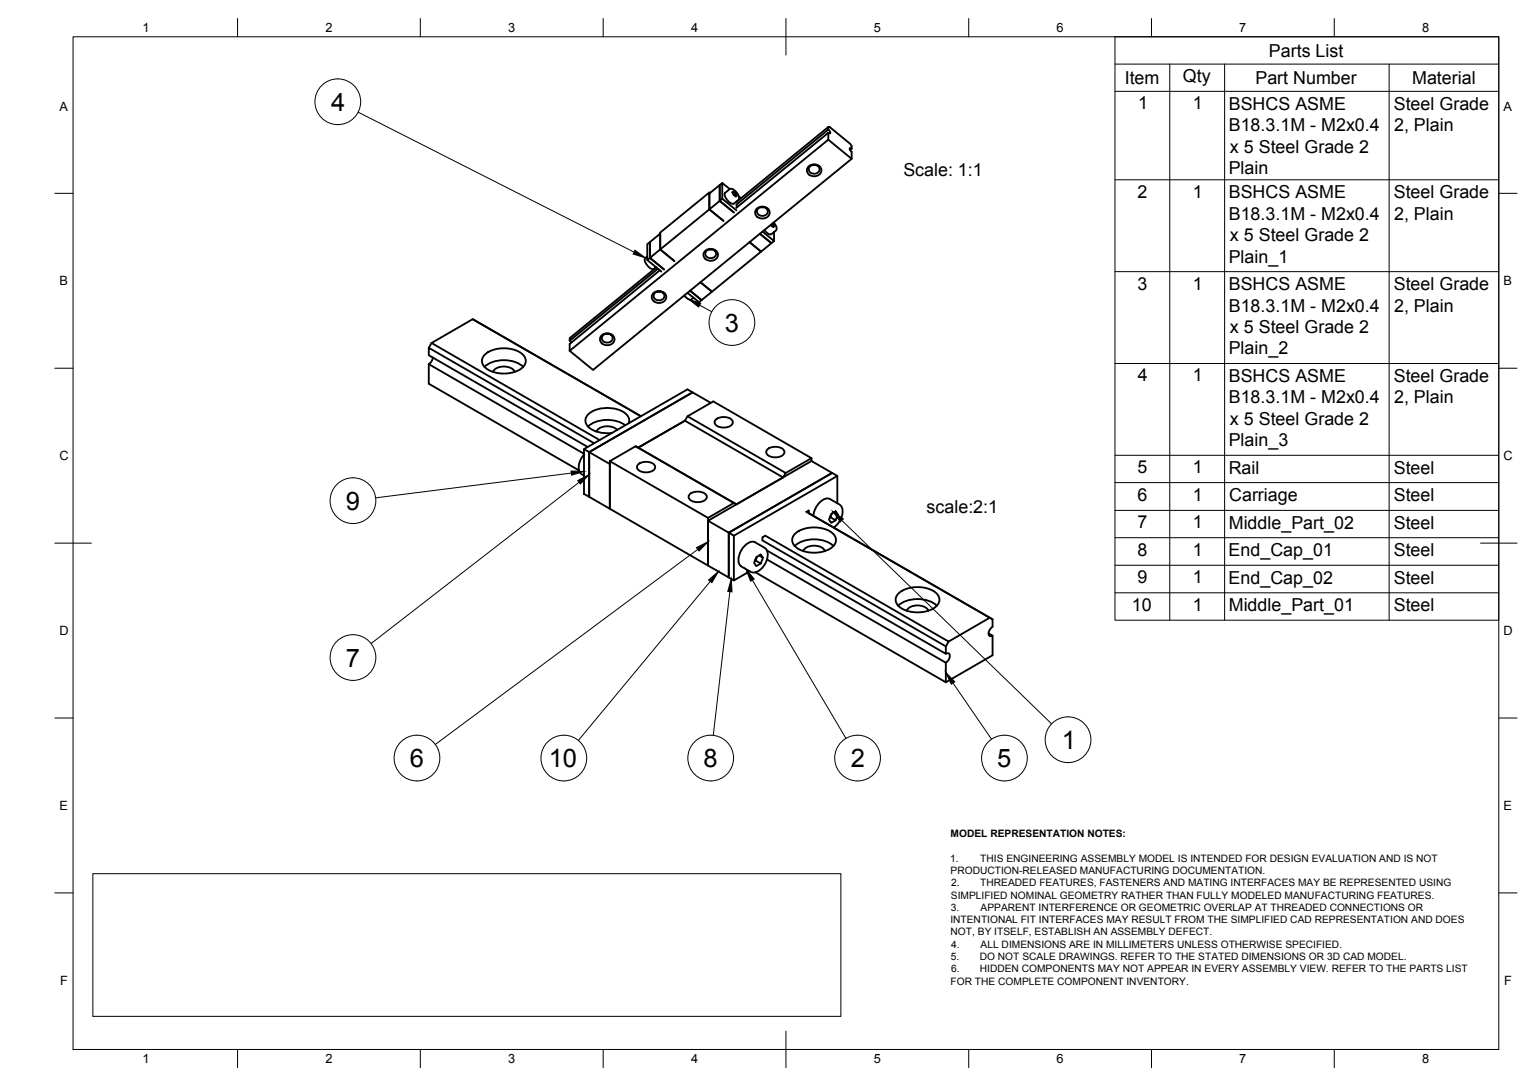
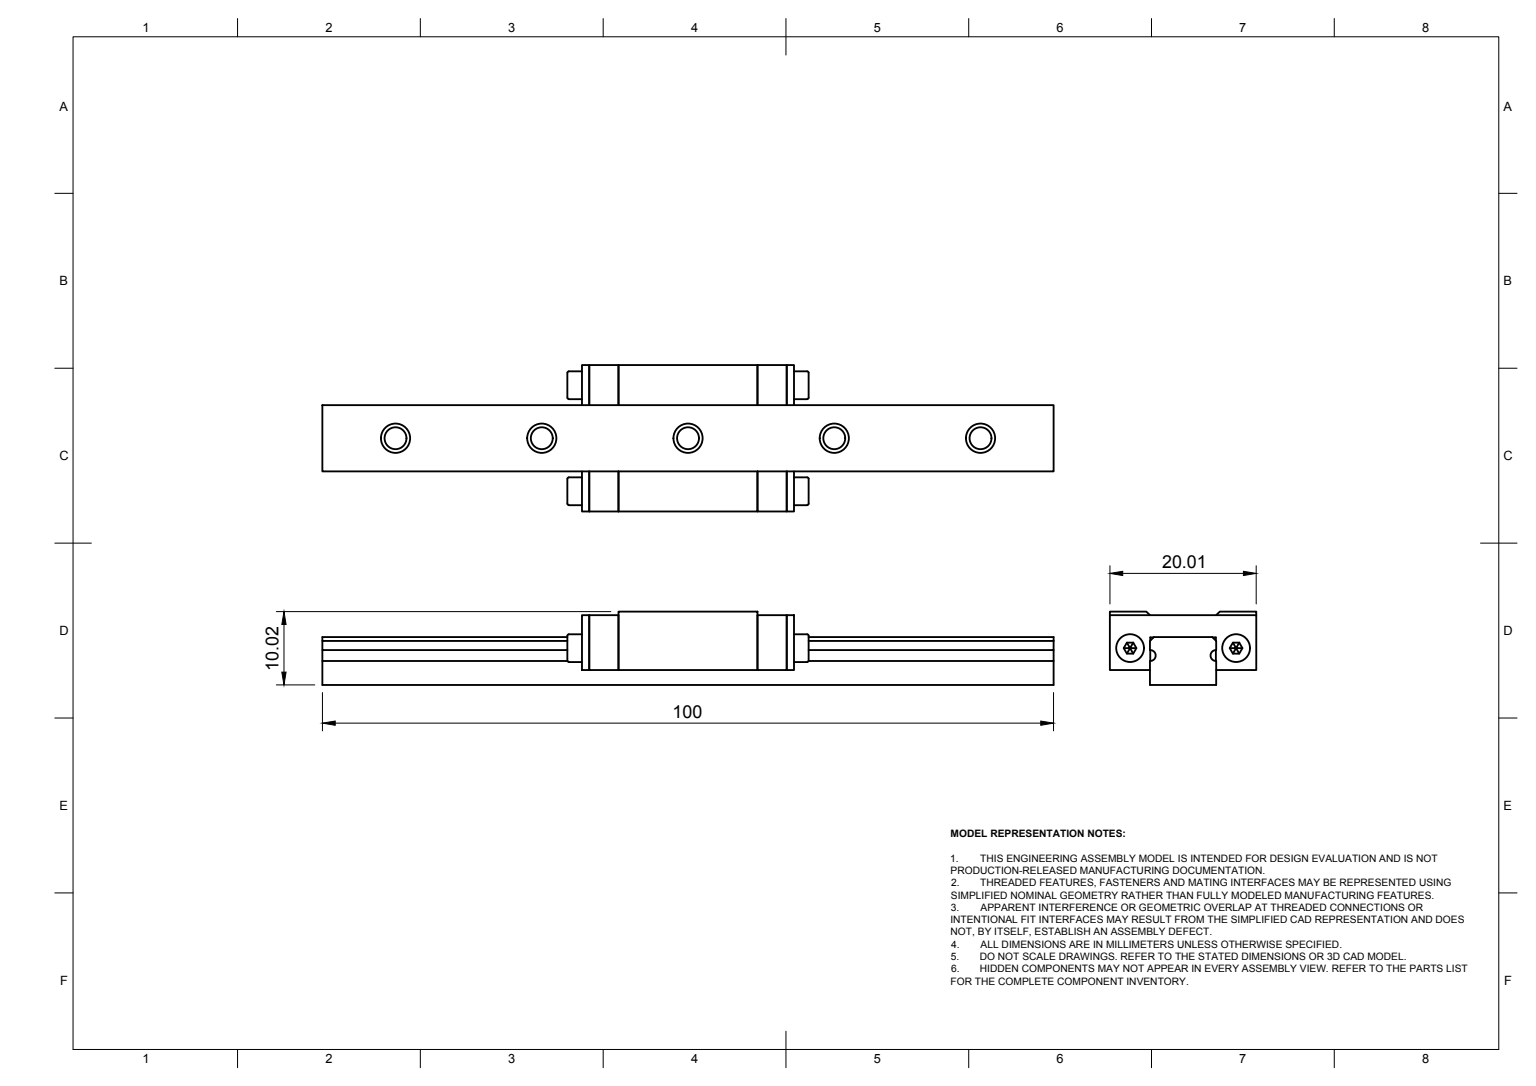
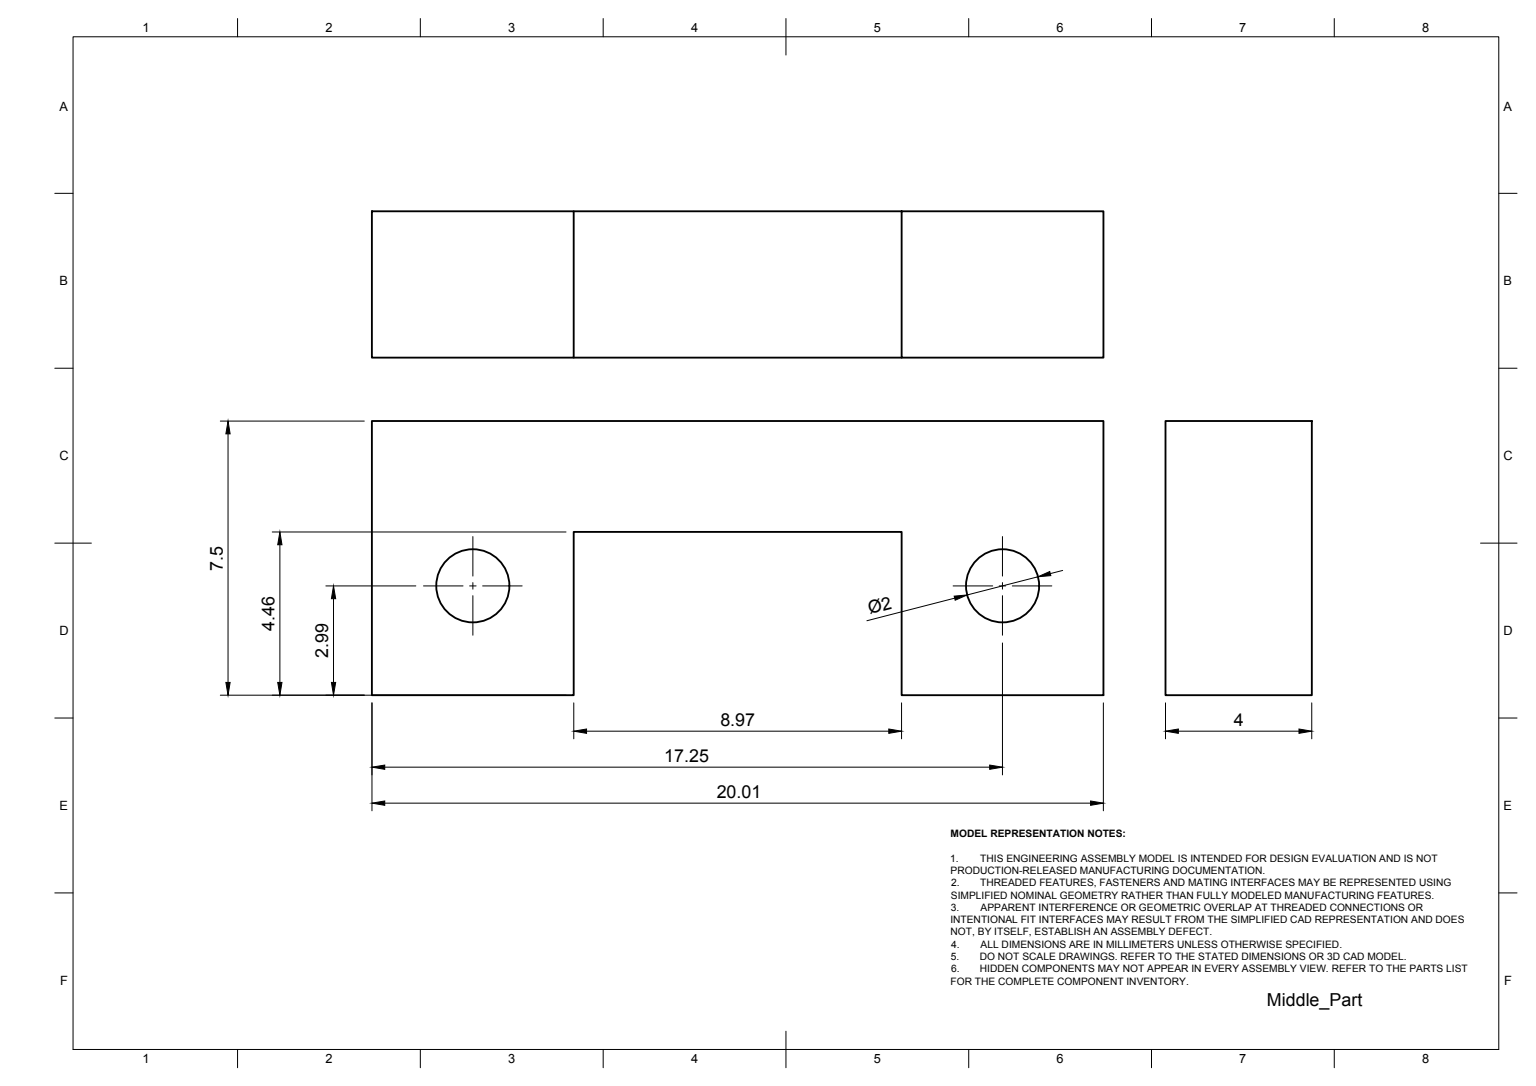
ISO-10303-21;
HEADER;
/* Generated by software containing ST-Developer
 * from STEP Tools, Inc. (www.steptools.com) 
 */

FILE_DESCRIPTION(
/* description */ (''),
/* implementation_level */ '2;1');

FILE_NAME(
/* name */ 'BR-352',
/* time_stamp */ '2026-10-06T13:23:02-07:00',
/* author */ (''),
/* organization */ (''),
/* preprocessor_version */ 'ST-DEVELOPER v20.2',
/* originating_system */ 'Autodesk Translation Framework v15.15.0.0',
/* authorisation */ '');

FILE_SCHEMA (('AUTOMOTIVE_DESIGN { 1 0 10303 214 3 1 1 }'));
ENDSEC;

DATA;
#10=MECHANICAL_DESIGN_GEOMETRIC_PRESENTATION_REPRESENTATION('',(#71,#72,
#73,#74,#75,#76,#77,#78,#79,#80),#4994);
#11=ITEM_DEFINED_TRANSFORMATION($,$,#3033,#3302);
#12=ITEM_DEFINED_TRANSFORMATION($,$,#3060,#3303);
#13=ITEM_DEFINED_TRANSFORMATION($,$,#3087,#3304);
#14=ITEM_DEFINED_TRANSFORMATION($,$,#3114,#3305);
#15=ITEM_DEFINED_TRANSFORMATION($,$,#3141,#3306);
#16=ITEM_DEFINED_TRANSFORMATION($,$,#3203,#3307);
#17=ITEM_DEFINED_TRANSFORMATION($,$,#3234,#3308);
#18=ITEM_DEFINED_TRANSFORMATION($,$,#3251,#3309);
#19=ITEM_DEFINED_TRANSFORMATION($,$,#3268,#3310);
#20=ITEM_DEFINED_TRANSFORMATION($,$,#3285,#3311);
#21=(
REPRESENTATION_RELATIONSHIP($,$,#5032,#5031)
REPRESENTATION_RELATIONSHIP_WITH_TRANSFORMATION(#11)
SHAPE_REPRESENTATION_RELATIONSHIP()
);
#22=(
REPRESENTATION_RELATIONSHIP($,$,#5033,#5031)
REPRESENTATION_RELATIONSHIP_WITH_TRANSFORMATION(#12)
SHAPE_REPRESENTATION_RELATIONSHIP()
);
#23=(
REPRESENTATION_RELATIONSHIP($,$,#5034,#5031)
REPRESENTATION_RELATIONSHIP_WITH_TRANSFORMATION(#13)
SHAPE_REPRESENTATION_RELATIONSHIP()
);
#24=(
REPRESENTATION_RELATIONSHIP($,$,#5035,#5031)
REPRESENTATION_RELATIONSHIP_WITH_TRANSFORMATION(#14)
SHAPE_REPRESENTATION_RELATIONSHIP()
);
#25=(
REPRESENTATION_RELATIONSHIP($,$,#5036,#5031)
REPRESENTATION_RELATIONSHIP_WITH_TRANSFORMATION(#15)
SHAPE_REPRESENTATION_RELATIONSHIP()
);
#26=(
REPRESENTATION_RELATIONSHIP($,$,#5037,#5031)
REPRESENTATION_RELATIONSHIP_WITH_TRANSFORMATION(#16)
SHAPE_REPRESENTATION_RELATIONSHIP()
);
#27=(
REPRESENTATION_RELATIONSHIP($,$,#5038,#5031)
REPRESENTATION_RELATIONSHIP_WITH_TRANSFORMATION(#17)
SHAPE_REPRESENTATION_RELATIONSHIP()
);
#28=(
REPRESENTATION_RELATIONSHIP($,$,#5039,#5031)
REPRESENTATION_RELATIONSHIP_WITH_TRANSFORMATION(#18)
SHAPE_REPRESENTATION_RELATIONSHIP()
);
#29=(
REPRESENTATION_RELATIONSHIP($,$,#5040,#5031)
REPRESENTATION_RELATIONSHIP_WITH_TRANSFORMATION(#19)
SHAPE_REPRESENTATION_RELATIONSHIP()
);
#30=(
REPRESENTATION_RELATIONSHIP($,$,#5041,#5031)
REPRESENTATION_RELATIONSHIP_WITH_TRANSFORMATION(#20)
SHAPE_REPRESENTATION_RELATIONSHIP()
);
#31=CONTEXT_DEPENDENT_SHAPE_REPRESENTATION(#21,#5021);
#32=CONTEXT_DEPENDENT_SHAPE_REPRESENTATION(#22,#5022);
#33=CONTEXT_DEPENDENT_SHAPE_REPRESENTATION(#23,#5023);
#34=CONTEXT_DEPENDENT_SHAPE_REPRESENTATION(#24,#5024);
#35=CONTEXT_DEPENDENT_SHAPE_REPRESENTATION(#25,#5025);
#36=CONTEXT_DEPENDENT_SHAPE_REPRESENTATION(#26,#5026);
#37=CONTEXT_DEPENDENT_SHAPE_REPRESENTATION(#27,#5027);
#38=CONTEXT_DEPENDENT_SHAPE_REPRESENTATION(#28,#5028);
#39=CONTEXT_DEPENDENT_SHAPE_REPRESENTATION(#29,#5029);
#40=CONTEXT_DEPENDENT_SHAPE_REPRESENTATION(#30,#5030);
#41=NEXT_ASSEMBLY_USAGE_OCCURRENCE('Screw_01:1','Screw_01:1',
'Screw_01:1',#5043,#5044,'Screw_01:1');
#42=NEXT_ASSEMBLY_USAGE_OCCURRENCE('Screw_02:1','Screw_02:1',
'Screw_02:1',#5043,#5045,'Screw_02:1');
#43=NEXT_ASSEMBLY_USAGE_OCCURRENCE('Screw_03:1','Screw_03:1',
'Screw_03:1',#5043,#5046,'Screw_03:1');
#44=NEXT_ASSEMBLY_USAGE_OCCURRENCE('Screw_04:1','Screw_04:1',
'Screw_04:1',#5043,#5047,'Screw_04:1');
#45=NEXT_ASSEMBLY_USAGE_OCCURRENCE('Rail:1','Rail:1','Rail:1',#5043,#5048,
'Rail:1');
#46=NEXT_ASSEMBLY_USAGE_OCCURRENCE('Carriage:1','Carriage:1',
'Carriage:1',#5043,#5049,'Carriage:1');
#47=NEXT_ASSEMBLY_USAGE_OCCURRENCE('Middle_Part_02:1',
'Middle_Part_02:1','Middle_Part_02:1',#5043,#5050,'Middle_Part_02:1');
#48=NEXT_ASSEMBLY_USAGE_OCCURRENCE('End_Cap_01:1','End_Cap_01:1',
'End_Cap_01:1',#5043,#5051,'End_Cap_01:1');
#49=NEXT_ASSEMBLY_USAGE_OCCURRENCE('End_Cap_02:1','End_Cap_02:1',
'End_Cap_02:1',#5043,#5052,'End_Cap_02:1');
#50=NEXT_ASSEMBLY_USAGE_OCCURRENCE('Middle_Part_01:1',
'Middle_Part_01:1','Middle_Part_01:1',#5043,#5053,'Middle_Part_01:1');
#51=SHAPE_REPRESENTATION_RELATIONSHIP('SRR','None',#5032,#61);
#52=SHAPE_REPRESENTATION_RELATIONSHIP('SRR','None',#5033,#62);
#53=SHAPE_REPRESENTATION_RELATIONSHIP('SRR','None',#5034,#63);
#54=SHAPE_REPRESENTATION_RELATIONSHIP('SRR','None',#5035,#64);
#55=SHAPE_REPRESENTATION_RELATIONSHIP('SRR','None',#5036,#65);
#56=SHAPE_REPRESENTATION_RELATIONSHIP('SRR','None',#5037,#66);
#57=SHAPE_REPRESENTATION_RELATIONSHIP('SRR','None',#5038,#67);
#58=SHAPE_REPRESENTATION_RELATIONSHIP('SRR','None',#5039,#68);
#59=SHAPE_REPRESENTATION_RELATIONSHIP('SRR','None',#5040,#69);
#60=SHAPE_REPRESENTATION_RELATIONSHIP('SRR','None',#5041,#70);
#61=ADVANCED_BREP_SHAPE_REPRESENTATION('',(#81),#4984);
#62=ADVANCED_BREP_SHAPE_REPRESENTATION('',(#82),#4985);
#63=ADVANCED_BREP_SHAPE_REPRESENTATION('',(#83),#4986);
#64=ADVANCED_BREP_SHAPE_REPRESENTATION('',(#84),#4987);
#65=ADVANCED_BREP_SHAPE_REPRESENTATION('',(#85),#4988);
#66=ADVANCED_BREP_SHAPE_REPRESENTATION('',(#86),#4989);
#67=ADVANCED_BREP_SHAPE_REPRESENTATION('',(#87),#4990);
#68=ADVANCED_BREP_SHAPE_REPRESENTATION('',(#88),#4991);
#69=ADVANCED_BREP_SHAPE_REPRESENTATION('',(#89),#4992);
#70=ADVANCED_BREP_SHAPE_REPRESENTATION('',(#90),#4993);
#71=STYLED_ITEM('',(#5091),#81);
#72=STYLED_ITEM('',(#5091),#82);
#73=STYLED_ITEM('',(#5091),#83);
#74=STYLED_ITEM('',(#5091),#84);
#75=STYLED_ITEM('',(#5092),#85);
#76=STYLED_ITEM('',(#5092),#86);
#77=STYLED_ITEM('',(#5093),#87);
#78=STYLED_ITEM('',(#5094),#88);
#79=STYLED_ITEM('',(#5094),#89);
#80=STYLED_ITEM('',(#5093),#90);
#81=MANIFOLD_SOLID_BREP('Body1',#2911);
#82=MANIFOLD_SOLID_BREP('Body1',#2912);
#83=MANIFOLD_SOLID_BREP('Body1',#2913);
#84=MANIFOLD_SOLID_BREP('Body1',#2914);
#85=MANIFOLD_SOLID_BREP('Body1',#2915);
#86=MANIFOLD_SOLID_BREP('Body1',#2916);
#87=MANIFOLD_SOLID_BREP('Body1',#2917);
#88=MANIFOLD_SOLID_BREP('Body1',#2918);
#89=MANIFOLD_SOLID_BREP('Body1',#2919);
#90=MANIFOLD_SOLID_BREP('Body1',#2920);
#91=CYLINDRICAL_SURFACE('',#3042,1.9);
#92=CYLINDRICAL_SURFACE('',#3056,0.96675);
#93=CYLINDRICAL_SURFACE('',#3069,1.9);
#94=CYLINDRICAL_SURFACE('',#3083,0.96675);
#95=CYLINDRICAL_SURFACE('',#3096,1.9);
#96=CYLINDRICAL_SURFACE('',#3110,0.96675);
#97=CYLINDRICAL_SURFACE('',#3123,1.9);
#98=CYLINDRICAL_SURFACE('',#3137,0.96675);
#99=CYLINDRICAL_SURFACE('',#3150,1.5);
#100=CYLINDRICAL_SURFACE('',#3154,1.5);
#101=CYLINDRICAL_SURFACE('',#3158,1.5);
#102=CYLINDRICAL_SURFACE('',#3162,1.5);
#103=CYLINDRICAL_SURFACE('',#3166,1.5);
#104=CYLINDRICAL_SURFACE('',#3168,3.);
#105=CYLINDRICAL_SURFACE('',#3172,3.);
#106=CYLINDRICAL_SURFACE('',#3176,3.);
#107=CYLINDRICAL_SURFACE('',#3180,3.);
#108=CYLINDRICAL_SURFACE('',#3184,3.);
#109=CYLINDRICAL_SURFACE('',#3189,0.747295203682);
#110=CYLINDRICAL_SURFACE('',#3197,0.747295203682);
#111=CYLINDRICAL_SURFACE('',#3204,1.25);
#112=CYLINDRICAL_SURFACE('',#3208,1.25);
#113=CYLINDRICAL_SURFACE('',#3212,1.25);
#114=CYLINDRICAL_SURFACE('',#3216,1.25);
#115=CYLINDRICAL_SURFACE('',#3235,1.);
#116=CYLINDRICAL_SURFACE('',#3238,1.);
#117=CYLINDRICAL_SURFACE('',#3252,1.);
#118=CYLINDRICAL_SURFACE('',#3255,1.);
#119=CYLINDRICAL_SURFACE('',#3269,1.);
#120=CYLINDRICAL_SURFACE('',#3272,1.);
#121=CYLINDRICAL_SURFACE('',#3286,1.);
#122=CYLINDRICAL_SURFACE('',#3289,1.);
#123=FACE_BOUND('',#484,.T.);
#124=FACE_BOUND('',#501,.T.);
#125=FACE_BOUND('',#505,.T.);
#126=FACE_BOUND('',#522,.T.);
#127=FACE_BOUND('',#526,.T.);
#128=FACE_BOUND('',#543,.T.);
#129=FACE_BOUND('',#547,.T.);
#130=FACE_BOUND('',#564,.T.);
#131=FACE_BOUND('',#567,.T.);
#132=FACE_BOUND('',#568,.T.);
#133=FACE_BOUND('',#569,.T.);
#134=FACE_BOUND('',#570,.T.);
#135=FACE_BOUND('',#571,.T.);
#136=FACE_BOUND('',#583,.T.);
#137=FACE_BOUND('',#586,.T.);
#138=FACE_BOUND('',#589,.T.);
#139=FACE_BOUND('',#592,.T.);
#140=FACE_BOUND('',#595,.T.);
#141=FACE_BOUND('',#605,.T.);
#142=FACE_BOUND('',#606,.T.);
#143=FACE_BOUND('',#607,.T.);
#144=FACE_BOUND('',#608,.T.);
#145=FACE_BOUND('',#609,.T.);
#146=FACE_BOUND('',#625,.T.);
#147=FACE_BOUND('',#626,.T.);
#148=FACE_BOUND('',#631,.T.);
#149=FACE_BOUND('',#632,.T.);
#150=FACE_BOUND('',#649,.T.);
#151=FACE_BOUND('',#650,.T.);
#152=FACE_BOUND('',#652,.T.);
#153=FACE_BOUND('',#653,.T.);
#154=FACE_BOUND('',#665,.T.);
#155=FACE_BOUND('',#666,.T.);
#156=FACE_BOUND('',#668,.T.);
#157=FACE_BOUND('',#669,.T.);
#158=FACE_BOUND('',#681,.T.);
#159=FACE_BOUND('',#682,.T.);
#160=FACE_BOUND('',#684,.T.);
#161=FACE_BOUND('',#685,.T.);
#162=FACE_BOUND('',#697,.T.);
#163=FACE_BOUND('',#698,.T.);
#164=FACE_BOUND('',#700,.T.);
#165=FACE_BOUND('',#701,.T.);
#166=PLANE('',#3041);
#167=PLANE('',#3044);
#168=PLANE('',#3045);
#169=PLANE('',#3046);
#170=PLANE('',#3047);
#171=PLANE('',#3048);
#172=PLANE('',#3049);
#173=PLANE('',#3050);
#174=PLANE('',#3051);
#175=PLANE('',#3052);
#176=PLANE('',#3053);
#177=PLANE('',#3054);
#178=PLANE('',#3055);
#179=PLANE('',#3058);
#180=PLANE('',#3059);
#181=PLANE('',#3068);
#182=PLANE('',#3071);
#183=PLANE('',#3072);
#184=PLANE('',#3073);
#185=PLANE('',#3074);
#186=PLANE('',#3075);
#187=PLANE('',#3076);
#188=PLANE('',#3077);
#189=PLANE('',#3078);
#190=PLANE('',#3079);
#191=PLANE('',#3080);
#192=PLANE('',#3081);
#193=PLANE('',#3082);
#194=PLANE('',#3085);
#195=PLANE('',#3086);
#196=PLANE('',#3095);
#197=PLANE('',#3098);
#198=PLANE('',#3099);
#199=PLANE('',#3100);
#200=PLANE('',#3101);
#201=PLANE('',#3102);
#202=PLANE('',#3103);
#203=PLANE('',#3104);
#204=PLANE('',#3105);
#205=PLANE('',#3106);
#206=PLANE('',#3107);
#207=PLANE('',#3108);
#208=PLANE('',#3109);
#209=PLANE('',#3112);
#210=PLANE('',#3113);
#211=PLANE('',#3122);
#212=PLANE('',#3125);
#213=PLANE('',#3126);
#214=PLANE('',#3127);
#215=PLANE('',#3128);
#216=PLANE('',#3129);
#217=PLANE('',#3130);
#218=PLANE('',#3131);
#219=PLANE('',#3132);
#220=PLANE('',#3133);
#221=PLANE('',#3134);
#222=PLANE('',#3135);
#223=PLANE('',#3136);
#224=PLANE('',#3139);
#225=PLANE('',#3140);
#226=PLANE('',#3145);
#227=PLANE('',#3171);
#228=PLANE('',#3175);
#229=PLANE('',#3179);
#230=PLANE('',#3183);
#231=PLANE('',#3187);
#232=PLANE('',#3188);
#233=PLANE('',#3192);
#234=PLANE('',#3193);
#235=PLANE('',#3194);
#236=PLANE('',#3196);
#237=PLANE('',#3199);
#238=PLANE('',#3200);
#239=PLANE('',#3201);
#240=PLANE('',#3202);
#241=PLANE('',#3207);
#242=PLANE('',#3211);
#243=PLANE('',#3215);
#244=PLANE('',#3219);
#245=PLANE('',#3220);
#246=PLANE('',#3221);
#247=PLANE('',#3222);
#248=PLANE('',#3223);
#249=PLANE('',#3224);
#250=PLANE('',#3225);
#251=PLANE('',#3226);
#252=PLANE('',#3227);
#253=PLANE('',#3228);
#254=PLANE('',#3229);
#255=PLANE('',#3230);
#256=PLANE('',#3231);
#257=PLANE('',#3232);
#258=PLANE('',#3233);
#259=PLANE('',#3241);
#260=PLANE('',#3242);
#261=PLANE('',#3243);
#262=PLANE('',#3244);
#263=PLANE('',#3245);
#264=PLANE('',#3246);
#265=PLANE('',#3247);
#266=PLANE('',#3248);
#267=PLANE('',#3249);
#268=PLANE('',#3250);
#269=PLANE('',#3258);
#270=PLANE('',#3259);
#271=PLANE('',#3260);
#272=PLANE('',#3261);
#273=PLANE('',#3262);
#274=PLANE('',#3263);
#275=PLANE('',#3264);
#276=PLANE('',#3265);
#277=PLANE('',#3266);
#278=PLANE('',#3267);
#279=PLANE('',#3275);
#280=PLANE('',#3276);
#281=PLANE('',#3277);
#282=PLANE('',#3278);
#283=PLANE('',#3279);
#284=PLANE('',#3280);
#285=PLANE('',#3281);
#286=PLANE('',#3282);
#287=PLANE('',#3283);
#288=PLANE('',#3284);
#289=PLANE('',#3292);
#290=PLANE('',#3293);
#291=PLANE('',#3294);
#292=PLANE('',#3295);
#293=PLANE('',#3296);
#294=PLANE('',#3297);
#295=PLANE('',#3298);
#296=PLANE('',#3299);
#297=PLANE('',#3300);
#298=PLANE('',#3301);
#299=TOROIDAL_SURFACE('',#3037,1.7,0.2);
#300=TOROIDAL_SURFACE('',#3064,1.7,0.2);
#301=TOROIDAL_SURFACE('',#3091,1.7,0.2);
#302=TOROIDAL_SURFACE('',#3118,1.7,0.2);
#303=FACE_OUTER_BOUND('',#481,.T.);
#304=FACE_OUTER_BOUND('',#482,.T.);
#305=FACE_OUTER_BOUND('',#483,.T.);
#306=FACE_OUTER_BOUND('',#485,.T.);
#307=FACE_OUTER_BOUND('',#486,.T.);
#308=FACE_OUTER_BOUND('',#487,.T.);
#309=FACE_OUTER_BOUND('',#488,.T.);
#310=FACE_OUTER_BOUND('',#489,.T.);
#311=FACE_OUTER_BOUND('',#490,.T.);
#312=FACE_OUTER_BOUND('',#491,.T.);
#313=FACE_OUTER_BOUND('',#492,.T.);
#314=FACE_OUTER_BOUND('',#493,.T.);
#315=FACE_OUTER_BOUND('',#494,.T.);
#316=FACE_OUTER_BOUND('',#495,.T.);
#317=FACE_OUTER_BOUND('',#496,.T.);
#318=FACE_OUTER_BOUND('',#497,.T.);
#319=FACE_OUTER_BOUND('',#498,.T.);
#320=FACE_OUTER_BOUND('',#499,.T.);
#321=FACE_OUTER_BOUND('',#500,.T.);
#322=FACE_OUTER_BOUND('',#502,.T.);
#323=FACE_OUTER_BOUND('',#503,.T.);
#324=FACE_OUTER_BOUND('',#504,.T.);
#325=FACE_OUTER_BOUND('',#506,.T.);
#326=FACE_OUTER_BOUND('',#507,.T.);
#327=FACE_OUTER_BOUND('',#508,.T.);
#328=FACE_OUTER_BOUND('',#509,.T.);
#329=FACE_OUTER_BOUND('',#510,.T.);
#330=FACE_OUTER_BOUND('',#511,.T.);
#331=FACE_OUTER_BOUND('',#512,.T.);
#332=FACE_OUTER_BOUND('',#513,.T.);
#333=FACE_OUTER_BOUND('',#514,.T.);
#334=FACE_OUTER_BOUND('',#515,.T.);
#335=FACE_OUTER_BOUND('',#516,.T.);
#336=FACE_OUTER_BOUND('',#517,.T.);
#337=FACE_OUTER_BOUND('',#518,.T.);
#338=FACE_OUTER_BOUND('',#519,.T.);
#339=FACE_OUTER_BOUND('',#520,.T.);
#340=FACE_OUTER_BOUND('',#521,.T.);
#341=FACE_OUTER_BOUND('',#523,.T.);
#342=FACE_OUTER_BOUND('',#524,.T.);
#343=FACE_OUTER_BOUND('',#525,.T.);
#344=FACE_OUTER_BOUND('',#527,.T.);
#345=FACE_OUTER_BOUND('',#528,.T.);
#346=FACE_OUTER_BOUND('',#529,.T.);
#347=FACE_OUTER_BOUND('',#530,.T.);
#348=FACE_OUTER_BOUND('',#531,.T.);
#349=FACE_OUTER_BOUND('',#532,.T.);
#350=FACE_OUTER_BOUND('',#533,.T.);
#351=FACE_OUTER_BOUND('',#534,.T.);
#352=FACE_OUTER_BOUND('',#535,.T.);
#353=FACE_OUTER_BOUND('',#536,.T.);
#354=FACE_OUTER_BOUND('',#537,.T.);
#355=FACE_OUTER_BOUND('',#538,.T.);
#356=FACE_OUTER_BOUND('',#539,.T.);
#357=FACE_OUTER_BOUND('',#540,.T.);
#358=FACE_OUTER_BOUND('',#541,.T.);
#359=FACE_OUTER_BOUND('',#542,.T.);
#360=FACE_OUTER_BOUND('',#544,.T.);
#361=FACE_OUTER_BOUND('',#545,.T.);
#362=FACE_OUTER_BOUND('',#546,.T.);
#363=FACE_OUTER_BOUND('',#548,.T.);
#364=FACE_OUTER_BOUND('',#549,.T.);
#365=FACE_OUTER_BOUND('',#550,.T.);
#366=FACE_OUTER_BOUND('',#551,.T.);
#367=FACE_OUTER_BOUND('',#552,.T.);
#368=FACE_OUTER_BOUND('',#553,.T.);
#369=FACE_OUTER_BOUND('',#554,.T.);
#370=FACE_OUTER_BOUND('',#555,.T.);
#371=FACE_OUTER_BOUND('',#556,.T.);
#372=FACE_OUTER_BOUND('',#557,.T.);
#373=FACE_OUTER_BOUND('',#558,.T.);
#374=FACE_OUTER_BOUND('',#559,.T.);
#375=FACE_OUTER_BOUND('',#560,.T.);
#376=FACE_OUTER_BOUND('',#561,.T.);
#377=FACE_OUTER_BOUND('',#562,.T.);
#378=FACE_OUTER_BOUND('',#563,.T.);
#379=FACE_OUTER_BOUND('',#565,.T.);
#380=FACE_OUTER_BOUND('',#566,.T.);
#381=FACE_OUTER_BOUND('',#572,.T.);
#382=FACE_OUTER_BOUND('',#573,.T.);
#383=FACE_OUTER_BOUND('',#574,.T.);
#384=FACE_OUTER_BOUND('',#575,.T.);
#385=FACE_OUTER_BOUND('',#576,.T.);
#386=FACE_OUTER_BOUND('',#577,.T.);
#387=FACE_OUTER_BOUND('',#578,.T.);
#388=FACE_OUTER_BOUND('',#579,.T.);
#389=FACE_OUTER_BOUND('',#580,.T.);
#390=FACE_OUTER_BOUND('',#581,.T.);
#391=FACE_OUTER_BOUND('',#582,.T.);
#392=FACE_OUTER_BOUND('',#584,.T.);
#393=FACE_OUTER_BOUND('',#585,.T.);
#394=FACE_OUTER_BOUND('',#587,.T.);
#395=FACE_OUTER_BOUND('',#588,.T.);
#396=FACE_OUTER_BOUND('',#590,.T.);
#397=FACE_OUTER_BOUND('',#591,.T.);
#398=FACE_OUTER_BOUND('',#593,.T.);
#399=FACE_OUTER_BOUND('',#594,.T.);
#400=FACE_OUTER_BOUND('',#596,.T.);
#401=FACE_OUTER_BOUND('',#597,.T.);
#402=FACE_OUTER_BOUND('',#598,.T.);
#403=FACE_OUTER_BOUND('',#599,.T.);
#404=FACE_OUTER_BOUND('',#600,.T.);
#405=FACE_OUTER_BOUND('',#601,.T.);
#406=FACE_OUTER_BOUND('',#602,.T.);
#407=FACE_OUTER_BOUND('',#603,.T.);
#408=FACE_OUTER_BOUND('',#604,.T.);
#409=FACE_OUTER_BOUND('',#610,.T.);
#410=FACE_OUTER_BOUND('',#611,.T.);
#411=FACE_OUTER_BOUND('',#612,.T.);
#412=FACE_OUTER_BOUND('',#613,.T.);
#413=FACE_OUTER_BOUND('',#614,.T.);
#414=FACE_OUTER_BOUND('',#615,.T.);
#415=FACE_OUTER_BOUND('',#616,.T.);
#416=FACE_OUTER_BOUND('',#617,.T.);
#417=FACE_OUTER_BOUND('',#618,.T.);
#418=FACE_OUTER_BOUND('',#619,.T.);
#419=FACE_OUTER_BOUND('',#620,.T.);
#420=FACE_OUTER_BOUND('',#621,.T.);
#421=FACE_OUTER_BOUND('',#622,.T.);
#422=FACE_OUTER_BOUND('',#623,.T.);
#423=FACE_OUTER_BOUND('',#624,.T.);
#424=FACE_OUTER_BOUND('',#627,.T.);
#425=FACE_OUTER_BOUND('',#628,.T.);
#426=FACE_OUTER_BOUND('',#629,.T.);
#427=FACE_OUTER_BOUND('',#630,.T.);
#428=FACE_OUTER_BOUND('',#633,.T.);
#429=FACE_OUTER_BOUND('',#634,.T.);
#430=FACE_OUTER_BOUND('',#635,.T.);
#431=FACE_OUTER_BOUND('',#636,.T.);
#432=FACE_OUTER_BOUND('',#637,.T.);
#433=FACE_OUTER_BOUND('',#638,.T.);
#434=FACE_OUTER_BOUND('',#639,.T.);
#435=FACE_OUTER_BOUND('',#640,.T.);
#436=FACE_OUTER_BOUND('',#641,.T.);
#437=FACE_OUTER_BOUND('',#642,.T.);
#438=FACE_OUTER_BOUND('',#643,.T.);
#439=FACE_OUTER_BOUND('',#644,.T.);
#440=FACE_OUTER_BOUND('',#645,.T.);
#441=FACE_OUTER_BOUND('',#646,.T.);
#442=FACE_OUTER_BOUND('',#647,.T.);
#443=FACE_OUTER_BOUND('',#648,.T.);
#444=FACE_OUTER_BOUND('',#651,.T.);
#445=FACE_OUTER_BOUND('',#654,.T.);
#446=FACE_OUTER_BOUND('',#655,.T.);
#447=FACE_OUTER_BOUND('',#656,.T.);
#448=FACE_OUTER_BOUND('',#657,.T.);
#449=FACE_OUTER_BOUND('',#658,.T.);
#450=FACE_OUTER_BOUND('',#659,.T.);
#451=FACE_OUTER_BOUND('',#660,.T.);
#452=FACE_OUTER_BOUND('',#661,.T.);
#453=FACE_OUTER_BOUND('',#662,.T.);
#454=FACE_OUTER_BOUND('',#663,.T.);
#455=FACE_OUTER_BOUND('',#664,.T.);
#456=FACE_OUTER_BOUND('',#667,.T.);
#457=FACE_OUTER_BOUND('',#670,.T.);
#458=FACE_OUTER_BOUND('',#671,.T.);
#459=FACE_OUTER_BOUND('',#672,.T.);
#460=FACE_OUTER_BOUND('',#673,.T.);
#461=FACE_OUTER_BOUND('',#674,.T.);
#462=FACE_OUTER_BOUND('',#675,.T.);
#463=FACE_OUTER_BOUND('',#676,.T.);
#464=FACE_OUTER_BOUND('',#677,.T.);
#465=FACE_OUTER_BOUND('',#678,.T.);
#466=FACE_OUTER_BOUND('',#679,.T.);
#467=FACE_OUTER_BOUND('',#680,.T.);
#468=FACE_OUTER_BOUND('',#683,.T.);
#469=FACE_OUTER_BOUND('',#686,.T.);
#470=FACE_OUTER_BOUND('',#687,.T.);
#471=FACE_OUTER_BOUND('',#688,.T.);
#472=FACE_OUTER_BOUND('',#689,.T.);
#473=FACE_OUTER_BOUND('',#690,.T.);
#474=FACE_OUTER_BOUND('',#691,.T.);
#475=FACE_OUTER_BOUND('',#692,.T.);
#476=FACE_OUTER_BOUND('',#693,.T.);
#477=FACE_OUTER_BOUND('',#694,.T.);
#478=FACE_OUTER_BOUND('',#695,.T.);
#479=FACE_OUTER_BOUND('',#696,.T.);
#480=FACE_OUTER_BOUND('',#699,.T.);
#481=EDGE_LOOP('',(#1976,#1977,#1978,#1979));
#482=EDGE_LOOP('',(#1980,#1981,#1982,#1983));
#483=EDGE_LOOP('',(#1984));
#484=EDGE_LOOP('',(#1985,#1986,#1987,#1988,#1989,#1990));
#485=EDGE_LOOP('',(#1991,#1992,#1993,#1994));
#486=EDGE_LOOP('',(#1995,#1996,#1997));
#487=EDGE_LOOP('',(#1998,#1999,#2000));
#488=EDGE_LOOP('',(#2001,#2002,#2003));
#489=EDGE_LOOP('',(#2004,#2005,#2006));
#490=EDGE_LOOP('',(#2007,#2008,#2009));
#491=EDGE_LOOP('',(#2010,#2011,#2012));
#492=EDGE_LOOP('',(#2013,#2014,#2015,#2016));
#493=EDGE_LOOP('',(#2017,#2018,#2019,#2020));
#494=EDGE_LOOP('',(#2021,#2022,#2023,#2024));
#495=EDGE_LOOP('',(#2025,#2026,#2027,#2028));
#496=EDGE_LOOP('',(#2029,#2030,#2031,#2032));
#497=EDGE_LOOP('',(#2033,#2034,#2035,#2036));
#498=EDGE_LOOP('',(#2037,#2038,#2039,#2040));
#499=EDGE_LOOP('',(#2041));
#500=EDGE_LOOP('',(#2042));
#501=EDGE_LOOP('',(#2043));
#502=EDGE_LOOP('',(#2044,#2045,#2046,#2047));
#503=EDGE_LOOP('',(#2048,#2049,#2050,#2051));
#504=EDGE_LOOP('',(#2052));
#505=EDGE_LOOP('',(#2053,#2054,#2055,#2056,#2057,#2058));
#506=EDGE_LOOP('',(#2059,#2060,#2061,#2062));
#507=EDGE_LOOP('',(#2063,#2064,#2065));
#508=EDGE_LOOP('',(#2066,#2067,#2068));
#509=EDGE_LOOP('',(#2069,#2070,#2071));
#510=EDGE_LOOP('',(#2072,#2073,#2074));
#511=EDGE_LOOP('',(#2075,#2076,#2077));
#512=EDGE_LOOP('',(#2078,#2079,#2080));
#513=EDGE_LOOP('',(#2081,#2082,#2083,#2084));
#514=EDGE_LOOP('',(#2085,#2086,#2087,#2088));
#515=EDGE_LOOP('',(#2089,#2090,#2091,#2092));
#516=EDGE_LOOP('',(#2093,#2094,#2095,#2096));
#517=EDGE_LOOP('',(#2097,#2098,#2099,#2100));
#518=EDGE_LOOP('',(#2101,#2102,#2103,#2104));
#519=EDGE_LOOP('',(#2105,#2106,#2107,#2108));
#520=EDGE_LOOP('',(#2109));
#521=EDGE_LOOP('',(#2110));
#522=EDGE_LOOP('',(#2111));
#523=EDGE_LOOP('',(#2112,#2113,#2114,#2115));
#524=EDGE_LOOP('',(#2116,#2117,#2118,#2119));
#525=EDGE_LOOP('',(#2120));
#526=EDGE_LOOP('',(#2121,#2122,#2123,#2124,#2125,#2126));
#527=EDGE_LOOP('',(#2127,#2128,#2129,#2130));
#528=EDGE_LOOP('',(#2131,#2132,#2133));
#529=EDGE_LOOP('',(#2134,#2135,#2136));
#530=EDGE_LOOP('',(#2137,#2138,#2139));
#531=EDGE_LOOP('',(#2140,#2141,#2142));
#532=EDGE_LOOP('',(#2143,#2144,#2145));
#533=EDGE_LOOP('',(#2146,#2147,#2148));
#534=EDGE_LOOP('',(#2149,#2150,#2151,#2152));
#535=EDGE_LOOP('',(#2153,#2154,#2155,#2156));
#536=EDGE_LOOP('',(#2157,#2158,#2159,#2160));
#537=EDGE_LOOP('',(#2161,#2162,#2163,#2164));
#538=EDGE_LOOP('',(#2165,#2166,#2167,#2168));
#539=EDGE_LOOP('',(#2169,#2170,#2171,#2172));
#540=EDGE_LOOP('',(#2173,#2174,#2175,#2176));
#541=EDGE_LOOP('',(#2177));
#542=EDGE_LOOP('',(#2178));
#543=EDGE_LOOP('',(#2179));
#544=EDGE_LOOP('',(#2180,#2181,#2182,#2183));
#545=EDGE_LOOP('',(#2184,#2185,#2186,#2187));
#546=EDGE_LOOP('',(#2188));
#547=EDGE_LOOP('',(#2189,#2190,#2191,#2192,#2193,#2194));
#548=EDGE_LOOP('',(#2195,#2196,#2197,#2198));
#549=EDGE_LOOP('',(#2199,#2200,#2201));
#550=EDGE_LOOP('',(#2202,#2203,#2204));
#551=EDGE_LOOP('',(#2205,#2206,#2207));
#552=EDGE_LOOP('',(#2208,#2209,#2210));
#553=EDGE_LOOP('',(#2211,#2212,#2213));
#554=EDGE_LOOP('',(#2214,#2215,#2216));
#555=EDGE_LOOP('',(#2217,#2218,#2219,#2220));
#556=EDGE_LOOP('',(#2221,#2222,#2223,#2224));
#557=EDGE_LOOP('',(#2225,#2226,#2227,#2228));
#558=EDGE_LOOP('',(#2229,#2230,#2231,#2232));
#559=EDGE_LOOP('',(#2233,#2234,#2235,#2236));
#560=EDGE_LOOP('',(#2237,#2238,#2239,#2240));
#561=EDGE_LOOP('',(#2241,#2242,#2243,#2244));
#562=EDGE_LOOP('',(#2245));
#563=EDGE_LOOP('',(#2246));
#564=EDGE_LOOP('',(#2247));
#565=EDGE_LOOP('',(#2248,#2249,#2250,#2251));
#566=EDGE_LOOP('',(#2252,#2253,#2254,#2255));
#567=EDGE_LOOP('',(#2256));
#568=EDGE_LOOP('',(#2257));
#569=EDGE_LOOP('',(#2258));
#570=EDGE_LOOP('',(#2259));
#571=EDGE_LOOP('',(#2260));
#572=EDGE_LOOP('',(#2261,#2262,#2263,#2264));
#573=EDGE_LOOP('',(#2265,#2266,#2267,#2268));
#574=EDGE_LOOP('',(#2269,#2270,#2271,#2272));
#575=EDGE_LOOP('',(#2273,#2274,#2275,#2276));
#576=EDGE_LOOP('',(#2277,#2278,#2279,#2280));
#577=EDGE_LOOP('',(#2281,#2282,#2283,#2284));
#578=EDGE_LOOP('',(#2285,#2286,#2287,#2288));
#579=EDGE_LOOP('',(#2289,#2290,#2291,#2292));
#580=EDGE_LOOP('',(#2293,#2294,#2295,#2296));
#581=EDGE_LOOP('',(#2297,#2298,#2299,#2300));
#582=EDGE_LOOP('',(#2301));
#583=EDGE_LOOP('',(#2302));
#584=EDGE_LOOP('',(#2303,#2304,#2305,#2306));
#585=EDGE_LOOP('',(#2307));
#586=EDGE_LOOP('',(#2308));
#587=EDGE_LOOP('',(#2309,#2310,#2311,#2312));
#588=EDGE_LOOP('',(#2313));
#589=EDGE_LOOP('',(#2314));
#590=EDGE_LOOP('',(#2315,#2316,#2317,#2318));
#591=EDGE_LOOP('',(#2319));
#592=EDGE_LOOP('',(#2320));
#593=EDGE_LOOP('',(#2321,#2322,#2323,#2324));
#594=EDGE_LOOP('',(#2325));
#595=EDGE_LOOP('',(#2326));
#596=EDGE_LOOP('',(#2327,#2328,#2329,#2330));
#597=EDGE_LOOP('',(#2331,#2332,#2333,#2334));
#598=EDGE_LOOP('',(#2335,#2336,#2337,#2338));
#599=EDGE_LOOP('',(#2339,#2340,#2341,#2342));
#600=EDGE_LOOP('',(#2343,#2344,#2345,#2346,#2347,#2348,#2349,#2350,#2351,
#2352));
#601=EDGE_LOOP('',(#2353,#2354,#2355,#2356));
#602=EDGE_LOOP('',(#2357,#2358,#2359,#2360));
#603=EDGE_LOOP('',(#2361,#2362,#2363,#2364));
#604=EDGE_LOOP('',(#2365,#2366,#2367,#2368));
#605=EDGE_LOOP('',(#2369));
#606=EDGE_LOOP('',(#2370));
#607=EDGE_LOOP('',(#2371));
#608=EDGE_LOOP('',(#2372));
#609=EDGE_LOOP('',(#2373));
#610=EDGE_LOOP('',(#2374,#2375,#2376,#2377));
#611=EDGE_LOOP('',(#2378,#2379,#2380,#2381,#2382,#2383,#2384,#2385,#2386,
#2387));
#612=EDGE_LOOP('',(#2388,#2389,#2390,#2391));
#613=EDGE_LOOP('',(#2392));
#614=EDGE_LOOP('',(#2393,#2394,#2395,#2396));
#615=EDGE_LOOP('',(#2397));
#616=EDGE_LOOP('',(#2398,#2399,#2400,#2401));
#617=EDGE_LOOP('',(#2402));
#618=EDGE_LOOP('',(#2403,#2404,#2405,#2406));
#619=EDGE_LOOP('',(#2407));
#620=EDGE_LOOP('',(#2408,#2409,#2410,#2411,#2412,#2413,#2414,#2415,#2416,
#2417,#2418,#2419));
#621=EDGE_LOOP('',(#2420,#2421,#2422,#2423));
#622=EDGE_LOOP('',(#2424,#2425,#2426,#2427));
#623=EDGE_LOOP('',(#2428,#2429,#2430,#2431));
#624=EDGE_LOOP('',(#2432,#2433,#2434,#2435));
#625=EDGE_LOOP('',(#2436));
#626=EDGE_LOOP('',(#2437));
#627=EDGE_LOOP('',(#2438,#2439,#2440,#2441));
#628=EDGE_LOOP('',(#2442,#2443,#2444,#2445));
#629=EDGE_LOOP('',(#2446,#2447,#2448,#2449));
#630=EDGE_LOOP('',(#2450,#2451,#2452,#2453));
#631=EDGE_LOOP('',(#2454));
#632=EDGE_LOOP('',(#2455));
#633=EDGE_LOOP('',(#2456,#2457,#2458,#2459));
#634=EDGE_LOOP('',(#2460,#2461,#2462,#2463));
#635=EDGE_LOOP('',(#2464,#2465,#2466,#2467));
#636=EDGE_LOOP('',(#2468,#2469,#2470,#2471));
#637=EDGE_LOOP('',(#2472,#2473,#2474,#2475,#2476,#2477,#2478,#2479,#2480,
#2481,#2482,#2483));
#638=EDGE_LOOP('',(#2484,#2485,#2486,#2487));
#639=EDGE_LOOP('',(#2488,#2489,#2490,#2491));
#640=EDGE_LOOP('',(#2492,#2493,#2494,#2495));
#641=EDGE_LOOP('',(#2496,#2497,#2498,#2499));
#642=EDGE_LOOP('',(#2500,#2501,#2502,#2503));
#643=EDGE_LOOP('',(#2504,#2505,#2506,#2507));
#644=EDGE_LOOP('',(#2508,#2509,#2510,#2511));
#645=EDGE_LOOP('',(#2512,#2513,#2514,#2515));
#646=EDGE_LOOP('',(#2516,#2517,#2518,#2519));
#647=EDGE_LOOP('',(#2520,#2521,#2522,#2523));
#648=EDGE_LOOP('',(#2524,#2525,#2526,#2527,#2528,#2529,#2530,#2531));
#649=EDGE_LOOP('',(#2532));
#650=EDGE_LOOP('',(#2533));
#651=EDGE_LOOP('',(#2534,#2535,#2536,#2537,#2538,#2539,#2540,#2541));
#652=EDGE_LOOP('',(#2542));
#653=EDGE_LOOP('',(#2543));
#654=EDGE_LOOP('',(#2544,#2545,#2546,#2547));
#655=EDGE_LOOP('',(#2548,#2549,#2550,#2551));
#656=EDGE_LOOP('',(#2552,#2553,#2554,#2555));
#657=EDGE_LOOP('',(#2556,#2557,#2558,#2559));
#658=EDGE_LOOP('',(#2560,#2561,#2562,#2563));
#659=EDGE_LOOP('',(#2564,#2565,#2566,#2567));
#660=EDGE_LOOP('',(#2568,#2569,#2570,#2571));
#661=EDGE_LOOP('',(#2572,#2573,#2574,#2575));
#662=EDGE_LOOP('',(#2576,#2577,#2578,#2579));
#663=EDGE_LOOP('',(#2580,#2581,#2582,#2583));
#664=EDGE_LOOP('',(#2584,#2585,#2586,#2587,#2588,#2589,#2590,#2591));
#665=EDGE_LOOP('',(#2592));
#666=EDGE_LOOP('',(#2593));
#667=EDGE_LOOP('',(#2594,#2595,#2596,#2597,#2598,#2599,#2600,#2601));
#668=EDGE_LOOP('',(#2602));
#669=EDGE_LOOP('',(#2603));
#670=EDGE_LOOP('',(#2604,#2605,#2606,#2607));
#671=EDGE_LOOP('',(#2608,#2609,#2610,#2611));
#672=EDGE_LOOP('',(#2612,#2613,#2614,#2615));
#673=EDGE_LOOP('',(#2616,#2617,#2618,#2619));
#674=EDGE_LOOP('',(#2620,#2621,#2622,#2623));
#675=EDGE_LOOP('',(#2624,#2625,#2626,#2627));
#676=EDGE_LOOP('',(#2628,#2629,#2630,#2631));
#677=EDGE_LOOP('',(#2632,#2633,#2634,#2635));
#678=EDGE_LOOP('',(#2636,#2637,#2638,#2639));
#679=EDGE_LOOP('',(#2640,#2641,#2642,#2643));
#680=EDGE_LOOP('',(#2644,#2645,#2646,#2647,#2648,#2649,#2650,#2651));
#681=EDGE_LOOP('',(#2652));
#682=EDGE_LOOP('',(#2653));
#683=EDGE_LOOP('',(#2654,#2655,#2656,#2657,#2658,#2659,#2660,#2661));
#684=EDGE_LOOP('',(#2662));
#685=EDGE_LOOP('',(#2663));
#686=EDGE_LOOP('',(#2664,#2665,#2666,#2667));
#687=EDGE_LOOP('',(#2668,#2669,#2670,#2671));
#688=EDGE_LOOP('',(#2672,#2673,#2674,#2675));
#689=EDGE_LOOP('',(#2676,#2677,#2678,#2679));
#690=EDGE_LOOP('',(#2680,#2681,#2682,#2683));
#691=EDGE_LOOP('',(#2684,#2685,#2686,#2687));
#692=EDGE_LOOP('',(#2688,#2689,#2690,#2691));
#693=EDGE_LOOP('',(#2692,#2693,#2694,#2695));
#694=EDGE_LOOP('',(#2696,#2697,#2698,#2699));
#695=EDGE_LOOP('',(#2700,#2701,#2702,#2703));
#696=EDGE_LOOP('',(#2704,#2705,#2706,#2707,#2708,#2709,#2710,#2711));
#697=EDGE_LOOP('',(#2712));
#698=EDGE_LOOP('',(#2713));
#699=EDGE_LOOP('',(#2714,#2715,#2716,#2717,#2718,#2719,#2720,#2721));
#700=EDGE_LOOP('',(#2722));
#701=EDGE_LOOP('',(#2723));
#702=LINE('',#4171,#995);
#703=LINE('',#4182,#996);
#704=LINE('',#4184,#997);
#705=LINE('',#4186,#998);
#706=LINE('',#4188,#999);
#707=LINE('',#4190,#1000);
#708=LINE('',#4191,#1001);
#709=LINE('',#4195,#1002);
#710=LINE('',#4199,#1003);
#711=LINE('',#4201,#1004);
#712=LINE('',#4202,#1005);
#713=LINE('',#4205,#1006);
#714=LINE('',#4206,#1007);
#715=LINE('',#4209,#1008);
#716=LINE('',#4210,#1009);
#717=LINE('',#4213,#1010);
#718=LINE('',#4214,#1011);
#719=LINE('',#4217,#1012);
#720=LINE('',#4218,#1013);
#721=LINE('',#4220,#1014);
#722=LINE('',#4222,#1015);
#723=LINE('',#4223,#1016);
#724=LINE('',#4225,#1017);
#725=LINE('',#4227,#1018);
#726=LINE('',#4229,#1019);
#727=LINE('',#4231,#1020);
#728=LINE('',#4235,#1021);
#729=LINE('',#4244,#1022);
#730=LINE('',#4255,#1023);
#731=LINE('',#4257,#1024);
#732=LINE('',#4259,#1025);
#733=LINE('',#4261,#1026);
#734=LINE('',#4263,#1027);
#735=LINE('',#4264,#1028);
#736=LINE('',#4268,#1029);
#737=LINE('',#4272,#1030);
#738=LINE('',#4274,#1031);
#739=LINE('',#4275,#1032);
#740=LINE('',#4278,#1033);
#741=LINE('',#4279,#1034);
#742=LINE('',#4282,#1035);
#743=LINE('',#4283,#1036);
#744=LINE('',#4286,#1037);
#745=LINE('',#4287,#1038);
#746=LINE('',#4290,#1039);
#747=LINE('',#4291,#1040);
#748=LINE('',#4293,#1041);
#749=LINE('',#4295,#1042);
#750=LINE('',#4296,#1043);
#751=LINE('',#4298,#1044);
#752=LINE('',#4300,#1045);
#753=LINE('',#4302,#1046);
#754=LINE('',#4304,#1047);
#755=LINE('',#4308,#1048);
#756=LINE('',#4317,#1049);
#757=LINE('',#4328,#1050);
#758=LINE('',#4330,#1051);
#759=LINE('',#4332,#1052);
#760=LINE('',#4334,#1053);
#761=LINE('',#4336,#1054);
#762=LINE('',#4337,#1055);
#763=LINE('',#4341,#1056);
#764=LINE('',#4345,#1057);
#765=LINE('',#4347,#1058);
#766=LINE('',#4348,#1059);
#767=LINE('',#4351,#1060);
#768=LINE('',#4352,#1061);
#769=LINE('',#4355,#1062);
#770=LINE('',#4356,#1063);
#771=LINE('',#4359,#1064);
#772=LINE('',#4360,#1065);
#773=LINE('',#4363,#1066);
#774=LINE('',#4364,#1067);
#775=LINE('',#4366,#1068);
#776=LINE('',#4368,#1069);
#777=LINE('',#4369,#1070);
#778=LINE('',#4371,#1071);
#779=LINE('',#4373,#1072);
#780=LINE('',#4375,#1073);
#781=LINE('',#4377,#1074);
#782=LINE('',#4381,#1075);
#783=LINE('',#4390,#1076);
#784=LINE('',#4401,#1077);
#785=LINE('',#4403,#1078);
#786=LINE('',#4405,#1079);
#787=LINE('',#4407,#1080);
#788=LINE('',#4409,#1081);
#789=LINE('',#4410,#1082);
#790=LINE('',#4414,#1083);
#791=LINE('',#4418,#1084);
#792=LINE('',#4420,#1085);
#793=LINE('',#4421,#1086);
#794=LINE('',#4424,#1087);
#795=LINE('',#4425,#1088);
#796=LINE('',#4428,#1089);
#797=LINE('',#4429,#1090);
#798=LINE('',#4432,#1091);
#799=LINE('',#4433,#1092);
#800=LINE('',#4436,#1093);
#801=LINE('',#4437,#1094);
#802=LINE('',#4439,#1095);
#803=LINE('',#4441,#1096);
#804=LINE('',#4442,#1097);
#805=LINE('',#4444,#1098);
#806=LINE('',#4446,#1099);
#807=LINE('',#4448,#1100);
#808=LINE('',#4450,#1101);
#809=LINE('',#4454,#1102);
#810=LINE('',#4463,#1103);
#811=LINE('',#4468,#1104);
#812=LINE('',#4470,#1105);
#813=LINE('',#4472,#1106);
#814=LINE('',#4473,#1107);
#815=LINE('',#4485,#1108);
#816=LINE('',#4489,#1109);
#817=LINE('',#4493,#1110);
#818=LINE('',#4497,#1111);
#819=LINE('',#4501,#1112);
#820=LINE('',#4505,#1113);
#821=LINE('',#4509,#1114);
#822=LINE('',#4513,#1115);
#823=LINE('',#4517,#1116);
#824=LINE('',#4522,#1117);
#825=LINE('',#4529,#1118);
#826=LINE('',#4536,#1119);
#827=LINE('',#4543,#1120);
#828=LINE('',#4550,#1121);
#829=LINE('',#4556,#1122);
#830=LINE('',#4558,#1123);
#831=LINE('',#4560,#1124);
#832=LINE('',#4561,#1125);
#833=LINE('',#4566,#1126);
#834=LINE('',#4569,#1127);
#835=LINE('',#4570,#1128);
#836=LINE('',#4574,#1129);
#837=LINE('',#4575,#1130);
#838=LINE('',#4576,#1131);
#839=LINE('',#4580,#1132);
#840=LINE('',#4582,#1133);
#841=LINE('',#4585,#1134);
#842=LINE('',#4586,#1135);
#843=LINE('',#4589,#1136);
#844=LINE('',#4591,#1137);
#845=LINE('',#4592,#1138);
#846=LINE('',#4596,#1139);
#847=LINE('',#4598,#1140);
#848=LINE('',#4601,#1141);
#849=LINE('',#4602,#1142);
#850=LINE('',#4604,#1143);
#851=LINE('',#4611,#1144);
#852=LINE('',#4618,#1145);
#853=LINE('',#4625,#1146);
#854=LINE('',#4632,#1147);
#855=LINE('',#4638,#1148);
#856=LINE('',#4640,#1149);
#857=LINE('',#4642,#1150);
#858=LINE('',#4644,#1151);
#859=LINE('',#4646,#1152);
#860=LINE('',#4648,#1153);
#861=LINE('',#4650,#1154);
#862=LINE('',#4652,#1155);
#863=LINE('',#4654,#1156);
#864=LINE('',#4656,#1157);
#865=LINE('',#4658,#1158);
#866=LINE('',#4659,#1159);
#867=LINE('',#4662,#1160);
#868=LINE('',#4664,#1161);
#869=LINE('',#4665,#1162);
#870=LINE('',#4668,#1163);
#871=LINE('',#4669,#1164);
#872=LINE('',#4672,#1165);
#873=LINE('',#4673,#1166);
#874=LINE('',#4676,#1167);
#875=LINE('',#4677,#1168);
#876=LINE('',#4680,#1169);
#877=LINE('',#4681,#1170);
#878=LINE('',#4684,#1171);
#879=LINE('',#4685,#1172);
#880=LINE('',#4688,#1173);
#881=LINE('',#4689,#1174);
#882=LINE('',#4692,#1175);
#883=LINE('',#4693,#1176);
#884=LINE('',#4696,#1177);
#885=LINE('',#4697,#1178);
#886=LINE('',#4700,#1179);
#887=LINE('',#4701,#1180);
#888=LINE('',#4704,#1181);
#889=LINE('',#4705,#1182);
#890=LINE('',#4707,#1183);
#891=LINE('',#4714,#1184);
#892=LINE('',#4720,#1185);
#893=LINE('',#4725,#1186);
#894=LINE('',#4727,#1187);
#895=LINE('',#4729,#1188);
#896=LINE('',#4730,#1189);
#897=LINE('',#4733,#1190);
#898=LINE('',#4735,#1191);
#899=LINE('',#4736,#1192);
#900=LINE('',#4739,#1193);
#901=LINE('',#4741,#1194);
#902=LINE('',#4742,#1195);
#903=LINE('',#4745,#1196);
#904=LINE('',#4747,#1197);
#905=LINE('',#4748,#1198);
#906=LINE('',#4751,#1199);
#907=LINE('',#4753,#1200);
#908=LINE('',#4754,#1201);
#909=LINE('',#4757,#1202);
#910=LINE('',#4759,#1203);
#911=LINE('',#4760,#1204);
#912=LINE('',#4763,#1205);
#913=LINE('',#4765,#1206);
#914=LINE('',#4766,#1207);
#915=LINE('',#4768,#1208);
#916=LINE('',#4769,#1209);
#917=LINE('',#4777,#1210);
#918=LINE('',#4783,#1211);
#919=LINE('',#4788,#1212);
#920=LINE('',#4790,#1213);
#921=LINE('',#4792,#1214);
#922=LINE('',#4793,#1215);
#923=LINE('',#4796,#1216);
#924=LINE('',#4798,#1217);
#925=LINE('',#4799,#1218);
#926=LINE('',#4802,#1219);
#927=LINE('',#4804,#1220);
#928=LINE('',#4805,#1221);
#929=LINE('',#4808,#1222);
#930=LINE('',#4810,#1223);
#931=LINE('',#4811,#1224);
#932=LINE('',#4814,#1225);
#933=LINE('',#4816,#1226);
#934=LINE('',#4817,#1227);
#935=LINE('',#4820,#1228);
#936=LINE('',#4822,#1229);
#937=LINE('',#4823,#1230);
#938=LINE('',#4826,#1231);
#939=LINE('',#4828,#1232);
#940=LINE('',#4829,#1233);
#941=LINE('',#4831,#1234);
#942=LINE('',#4832,#1235);
#943=LINE('',#4840,#1236);
#944=LINE('',#4846,#1237);
#945=LINE('',#4851,#1238);
#946=LINE('',#4853,#1239);
#947=LINE('',#4855,#1240);
#948=LINE('',#4856,#1241);
#949=LINE('',#4859,#1242);
#950=LINE('',#4861,#1243);
#951=LINE('',#4862,#1244);
#952=LINE('',#4865,#1245);
#953=LINE('',#4867,#1246);
#954=LINE('',#4868,#1247);
#955=LINE('',#4871,#1248);
#956=LINE('',#4873,#1249);
#957=LINE('',#4874,#1250);
#958=LINE('',#4877,#1251);
#959=LINE('',#4879,#1252);
#960=LINE('',#4880,#1253);
#961=LINE('',#4883,#1254);
#962=LINE('',#4885,#1255);
#963=LINE('',#4886,#1256);
#964=LINE('',#4889,#1257);
#965=LINE('',#4891,#1258);
#966=LINE('',#4892,#1259);
#967=LINE('',#4894,#1260);
#968=LINE('',#4895,#1261);
#969=LINE('',#4903,#1262);
#970=LINE('',#4909,#1263);
#971=LINE('',#4914,#1264);
#972=LINE('',#4916,#1265);
#973=LINE('',#4918,#1266);
#974=LINE('',#4919,#1267);
#975=LINE('',#4922,#1268);
#976=LINE('',#4924,#1269);
#977=LINE('',#4925,#1270);
#978=LINE('',#4928,#1271);
#979=LINE('',#4930,#1272);
#980=LINE('',#4931,#1273);
#981=LINE('',#4934,#1274);
#982=LINE('',#4936,#1275);
#983=LINE('',#4937,#1276);
#984=LINE('',#4940,#1277);
#985=LINE('',#4942,#1278);
#986=LINE('',#4943,#1279);
#987=LINE('',#4946,#1280);
#988=LINE('',#4948,#1281);
#989=LINE('',#4949,#1282);
#990=LINE('',#4952,#1283);
#991=LINE('',#4954,#1284);
#992=LINE('',#4955,#1285);
#993=LINE('',#4957,#1286);
#994=LINE('',#4958,#1287);
#995=VECTOR('',#3320,0.887310000000001);
#996=VECTOR('',#3333,10.);
#997=VECTOR('',#3334,10.);
#998=VECTOR('',#3335,10.);
#999=VECTOR('',#3336,10.);
#1000=VECTOR('',#3337,10.);
#1001=VECTOR('',#3338,10.);
#1002=VECTOR('',#3343,1.9);
#1003=VECTOR('',#3346,9.99999999999999);
#1004=VECTOR('',#3347,10.);
#1005=VECTOR('',#3348,10.);
#1006=VECTOR('',#3351,10.);
#1007=VECTOR('',#3352,10.);
#1008=VECTOR('',#3355,10.);
#1009=VECTOR('',#3356,9.99999999999999);
#1010=VECTOR('',#3359,10.);
#1011=VECTOR('',#3360,10.);
#1012=VECTOR('',#3363,10.);
#1013=VECTOR('',#3364,10.);
#1014=VECTOR('',#3367,10.);
#1015=VECTOR('',#3370,10.);
#1016=VECTOR('',#3371,10.);
#1017=VECTOR('',#3374,10.);
#1018=VECTOR('',#3377,10.);
#1019=VECTOR('',#3380,10.);
#1020=VECTOR('',#3383,10.);
#1021=VECTOR('',#3388,0.96675);
#1022=VECTOR('',#3401,0.887310000000001);
#1023=VECTOR('',#3414,10.);
#1024=VECTOR('',#3415,10.);
#1025=VECTOR('',#3416,10.);
#1026=VECTOR('',#3417,10.);
#1027=VECTOR('',#3418,10.);
#1028=VECTOR('',#3419,10.);
#1029=VECTOR('',#3424,1.9);
#1030=VECTOR('',#3427,9.99999999999999);
#1031=VECTOR('',#3428,10.);
#1032=VECTOR('',#3429,10.);
#1033=VECTOR('',#3432,10.);
#1034=VECTOR('',#3433,10.);
#1035=VECTOR('',#3436,10.);
#1036=VECTOR('',#3437,9.99999999999999);
#1037=VECTOR('',#3440,10.);
#1038=VECTOR('',#3441,10.);
#1039=VECTOR('',#3444,10.);
#1040=VECTOR('',#3445,10.);
#1041=VECTOR('',#3448,10.);
#1042=VECTOR('',#3451,10.);
#1043=VECTOR('',#3452,10.);
#1044=VECTOR('',#3455,10.);
#1045=VECTOR('',#3458,10.);
#1046=VECTOR('',#3461,10.);
#1047=VECTOR('',#3464,10.);
#1048=VECTOR('',#3469,0.96675);
#1049=VECTOR('',#3482,0.887310000000001);
#1050=VECTOR('',#3495,10.);
#1051=VECTOR('',#3496,10.);
#1052=VECTOR('',#3497,10.);
#1053=VECTOR('',#3498,10.);
#1054=VECTOR('',#3499,10.);
#1055=VECTOR('',#3500,10.);
#1056=VECTOR('',#3505,1.9);
#1057=VECTOR('',#3508,9.99999999999999);
#1058=VECTOR('',#3509,10.);
#1059=VECTOR('',#3510,10.);
#1060=VECTOR('',#3513,10.);
#1061=VECTOR('',#3514,10.);
#1062=VECTOR('',#3517,10.);
#1063=VECTOR('',#3518,9.99999999999999);
#1064=VECTOR('',#3521,10.);
#1065=VECTOR('',#3522,10.);
#1066=VECTOR('',#3525,10.);
#1067=VECTOR('',#3526,10.);
#1068=VECTOR('',#3529,10.);
#1069=VECTOR('',#3532,10.);
#1070=VECTOR('',#3533,10.);
#1071=VECTOR('',#3536,10.);
#1072=VECTOR('',#3539,10.);
#1073=VECTOR('',#3542,10.);
#1074=VECTOR('',#3545,10.);
#1075=VECTOR('',#3550,0.96675);
#1076=VECTOR('',#3563,0.887310000000001);
#1077=VECTOR('',#3576,10.);
#1078=VECTOR('',#3577,10.);
#1079=VECTOR('',#3578,10.);
#1080=VECTOR('',#3579,10.);
#1081=VECTOR('',#3580,10.);
#1082=VECTOR('',#3581,10.);
#1083=VECTOR('',#3586,1.9);
#1084=VECTOR('',#3589,9.99999999999999);
#1085=VECTOR('',#3590,10.);
#1086=VECTOR('',#3591,10.);
#1087=VECTOR('',#3594,10.);
#1088=VECTOR('',#3595,10.);
#1089=VECTOR('',#3598,10.);
#1090=VECTOR('',#3599,9.99999999999999);
#1091=VECTOR('',#3602,10.);
#1092=VECTOR('',#3603,10.);
#1093=VECTOR('',#3606,10.);
#1094=VECTOR('',#3607,10.);
#1095=VECTOR('',#3610,10.);
#1096=VECTOR('',#3613,10.);
#1097=VECTOR('',#3614,10.);
#1098=VECTOR('',#3617,10.);
#1099=VECTOR('',#3620,10.);
#1100=VECTOR('',#3623,10.);
#1101=VECTOR('',#3626,10.);
#1102=VECTOR('',#3631,0.96675);
#1103=VECTOR('',#3644,1.75);
#1104=VECTOR('',#3649,10.);
#1105=VECTOR('',#3650,10.);
#1106=VECTOR('',#3651,10.);
#1107=VECTOR('',#3652,10.);
#1108=VECTOR('',#3665,1.5);
#1109=VECTOR('',#3670,1.75);
#1110=VECTOR('',#3675,1.5);
#1111=VECTOR('',#3680,1.75);
#1112=VECTOR('',#3685,1.5);
#1113=VECTOR('',#3690,1.75);
#1114=VECTOR('',#3695,1.5);
#1115=VECTOR('',#3700,1.75);
#1116=VECTOR('',#3705,1.5);
#1117=VECTOR('',#3710,3.);
#1118=VECTOR('',#3719,3.);
#1119=VECTOR('',#3728,3.);
#1120=VECTOR('',#3737,3.);
#1121=VECTOR('',#3746,3.);
#1122=VECTOR('',#3753,10.);
#1123=VECTOR('',#3754,10.);
#1124=VECTOR('',#3755,10.);
#1125=VECTOR('',#3756,10.);
#1126=VECTOR('',#3761,10.);
#1127=VECTOR('',#3766,10.);
#1128=VECTOR('',#3767,10.);
#1129=VECTOR('',#3770,10.);
#1130=VECTOR('',#3771,10.);
#1131=VECTOR('',#3772,10.);
#1132=VECTOR('',#3775,10.);
#1133=VECTOR('',#3776,10.);
#1134=VECTOR('',#3779,10.);
#1135=VECTOR('',#3780,10.);
#1136=VECTOR('',#3783,10.);
#1137=VECTOR('',#3784,10.);
#1138=VECTOR('',#3785,10.);
#1139=VECTOR('',#3790,10.);
#1140=VECTOR('',#3793,10.);
#1141=VECTOR('',#3796,10.);
#1142=VECTOR('',#3797,10.);
#1143=VECTOR('',#3800,10.);
#1144=VECTOR('',#3809,1.25);
#1145=VECTOR('',#3818,1.25);
#1146=VECTOR('',#3827,1.25);
#1147=VECTOR('',#3836,1.25);
#1148=VECTOR('',#3843,10.);
#1149=VECTOR('',#3844,10.);
#1150=VECTOR('',#3845,10.);
#1151=VECTOR('',#3846,10.);
#1152=VECTOR('',#3847,10.);
#1153=VECTOR('',#3848,10.);
#1154=VECTOR('',#3849,10.);
#1155=VECTOR('',#3850,10.);
#1156=VECTOR('',#3851,10.);
#1157=VECTOR('',#3852,10.);
#1158=VECTOR('',#3853,10.);
#1159=VECTOR('',#3854,10.);
#1160=VECTOR('',#3857,10.);
#1161=VECTOR('',#3858,10.);
#1162=VECTOR('',#3859,10.);
#1163=VECTOR('',#3862,10.);
#1164=VECTOR('',#3863,10.);
#1165=VECTOR('',#3866,10.);
#1166=VECTOR('',#3867,10.);
#1167=VECTOR('',#3870,10.);
#1168=VECTOR('',#3871,10.);
#1169=VECTOR('',#3874,10.);
#1170=VECTOR('',#3875,10.);
#1171=VECTOR('',#3878,10.);
#1172=VECTOR('',#3879,10.);
#1173=VECTOR('',#3882,10.);
#1174=VECTOR('',#3883,10.);
#1175=VECTOR('',#3886,10.);
#1176=VECTOR('',#3887,10.);
#1177=VECTOR('',#3890,10.);
#1178=VECTOR('',#3891,10.);
#1179=VECTOR('',#3894,10.);
#1180=VECTOR('',#3895,10.);
#1181=VECTOR('',#3898,10.);
#1182=VECTOR('',#3899,10.);
#1183=VECTOR('',#3902,10.);
#1184=VECTOR('',#3911,1.);
#1185=VECTOR('',#3918,1.);
#1186=VECTOR('',#3923,10.);
#1187=VECTOR('',#3924,10.);
#1188=VECTOR('',#3925,10.);
#1189=VECTOR('',#3926,10.);
#1190=VECTOR('',#3929,10.);
#1191=VECTOR('',#3930,10.);
#1192=VECTOR('',#3931,10.);
#1193=VECTOR('',#3934,10.);
#1194=VECTOR('',#3935,10.);
#1195=VECTOR('',#3936,10.);
#1196=VECTOR('',#3939,10.);
#1197=VECTOR('',#3940,10.);
#1198=VECTOR('',#3941,10.);
#1199=VECTOR('',#3944,10.);
#1200=VECTOR('',#3945,10.);
#1201=VECTOR('',#3946,10.);
#1202=VECTOR('',#3949,10.);
#1203=VECTOR('',#3950,10.);
#1204=VECTOR('',#3951,10.);
#1205=VECTOR('',#3954,10.);
#1206=VECTOR('',#3955,10.);
#1207=VECTOR('',#3956,10.);
#1208=VECTOR('',#3959,10.);
#1209=VECTOR('',#3960,10.);
#1210=VECTOR('',#3971,1.);
#1211=VECTOR('',#3978,1.);
#1212=VECTOR('',#3983,10.);
#1213=VECTOR('',#3984,10.);
#1214=VECTOR('',#3985,10.);
#1215=VECTOR('',#3986,10.);
#1216=VECTOR('',#3989,10.);
#1217=VECTOR('',#3990,10.);
#1218=VECTOR('',#3991,10.);
#1219=VECTOR('',#3994,10.);
#1220=VECTOR('',#3995,10.);
#1221=VECTOR('',#3996,10.);
#1222=VECTOR('',#3999,10.);
#1223=VECTOR('',#4000,10.);
#1224=VECTOR('',#4001,10.);
#1225=VECTOR('',#4004,10.);
#1226=VECTOR('',#4005,10.);
#1227=VECTOR('',#4006,10.);
#1228=VECTOR('',#4009,10.);
#1229=VECTOR('',#4010,10.);
#1230=VECTOR('',#4011,10.);
#1231=VECTOR('',#4014,10.);
#1232=VECTOR('',#4015,10.);
#1233=VECTOR('',#4016,10.);
#1234=VECTOR('',#4019,10.);
#1235=VECTOR('',#4020,10.);
#1236=VECTOR('',#4031,1.);
#1237=VECTOR('',#4038,1.);
#1238=VECTOR('',#4043,10.);
#1239=VECTOR('',#4044,10.);
#1240=VECTOR('',#4045,10.);
#1241=VECTOR('',#4046,10.);
#1242=VECTOR('',#4049,10.);
#1243=VECTOR('',#4050,10.);
#1244=VECTOR('',#4051,10.);
#1245=VECTOR('',#4054,10.);
#1246=VECTOR('',#4055,10.);
#1247=VECTOR('',#4056,10.);
#1248=VECTOR('',#4059,10.);
#1249=VECTOR('',#4060,10.);
#1250=VECTOR('',#4061,10.);
#1251=VECTOR('',#4064,10.);
#1252=VECTOR('',#4065,10.);
#1253=VECTOR('',#4066,10.);
#1254=VECTOR('',#4069,10.);
#1255=VECTOR('',#4070,10.);
#1256=VECTOR('',#4071,10.);
#1257=VECTOR('',#4074,10.);
#1258=VECTOR('',#4075,10.);
#1259=VECTOR('',#4076,10.);
#1260=VECTOR('',#4079,10.);
#1261=VECTOR('',#4080,10.);
#1262=VECTOR('',#4091,1.);
#1263=VECTOR('',#4098,1.);
#1264=VECTOR('',#4103,10.);
#1265=VECTOR('',#4104,10.);
#1266=VECTOR('',#4105,10.);
#1267=VECTOR('',#4106,10.);
#1268=VECTOR('',#4109,10.);
#1269=VECTOR('',#4110,10.);
#1270=VECTOR('',#4111,10.);
#1271=VECTOR('',#4114,10.);
#1272=VECTOR('',#4115,10.);
#1273=VECTOR('',#4116,10.);
#1274=VECTOR('',#4119,10.);
#1275=VECTOR('',#4120,10.);
#1276=VECTOR('',#4121,10.);
#1277=VECTOR('',#4124,10.);
#1278=VECTOR('',#4125,10.);
#1279=VECTOR('',#4126,10.);
#1280=VECTOR('',#4129,10.);
#1281=VECTOR('',#4130,10.);
#1282=VECTOR('',#4131,10.);
#1283=VECTOR('',#4134,10.);
#1284=VECTOR('',#4135,10.);
#1285=VECTOR('',#4136,10.);
#1286=VECTOR('',#4139,10.);
#1287=VECTOR('',#4140,10.);
#1288=CIRCLE('',#3035,0.96675);
#1289=CIRCLE('',#3036,0.754619999999998);
#1290=CIRCLE('',#3038,1.9);
#1291=CIRCLE('',#3039,0.2);
#1292=CIRCLE('',#3040,1.7);
#1293=CIRCLE('',#3043,1.9);
#1294=CIRCLE('',#3057,0.96675);
#1295=CIRCLE('',#3062,0.96675);
#1296=CIRCLE('',#3063,0.754619999999998);
#1297=CIRCLE('',#3065,1.9);
#1298=CIRCLE('',#3066,0.2);
#1299=CIRCLE('',#3067,1.7);
#1300=CIRCLE('',#3070,1.9);
#1301=CIRCLE('',#3084,0.96675);
#1302=CIRCLE('',#3089,0.96675);
#1303=CIRCLE('',#3090,0.754619999999998);
#1304=CIRCLE('',#3092,1.9);
#1305=CIRCLE('',#3093,0.2);
#1306=CIRCLE('',#3094,1.7);
#1307=CIRCLE('',#3097,1.9);
#1308=CIRCLE('',#3111,0.96675);
#1309=CIRCLE('',#3116,0.96675);
#1310=CIRCLE('',#3117,0.754619999999998);
#1311=CIRCLE('',#3119,1.9);
#1312=CIRCLE('',#3120,0.2);
#1313=CIRCLE('',#3121,1.7);
#1314=CIRCLE('',#3124,1.9);
#1315=CIRCLE('',#3138,0.96675);
#1316=CIRCLE('',#3143,1.5);
#1317=CIRCLE('',#3144,2.);
#1318=CIRCLE('',#3146,2.);
#1319=CIRCLE('',#3147,2.);
#1320=CIRCLE('',#3148,2.);
#1321=CIRCLE('',#3149,2.);
#1322=CIRCLE('',#3151,1.5);
#1323=CIRCLE('',#3153,1.5);
#1324=CIRCLE('',#3155,1.5);
#1325=CIRCLE('',#3157,1.5);
#1326=CIRCLE('',#3159,1.5);
#1327=CIRCLE('',#3161,1.5);
#1328=CIRCLE('',#3163,1.5);
#1329=CIRCLE('',#3165,1.5);
#1330=CIRCLE('',#3167,1.5);
#1331=CIRCLE('',#3169,3.);
#1332=CIRCLE('',#3170,3.);
#1333=CIRCLE('',#3173,3.);
#1334=CIRCLE('',#3174,3.);
#1335=CIRCLE('',#3177,3.);
#1336=CIRCLE('',#3178,3.);
#1337=CIRCLE('',#3181,3.);
#1338=CIRCLE('',#3182,3.);
#1339=CIRCLE('',#3185,3.);
#1340=CIRCLE('',#3186,3.);
#1341=CIRCLE('',#3190,0.747295203682);
#1342=CIRCLE('',#3191,0.747295203682);
#1343=CIRCLE('',#3195,0.747295203682);
#1344=CIRCLE('',#3198,0.747295203682);
#1345=CIRCLE('',#3205,1.25);
#1346=CIRCLE('',#3206,1.25);
#1347=CIRCLE('',#3209,1.25);
#1348=CIRCLE('',#3210,1.25);
#1349=CIRCLE('',#3213,1.25);
#1350=CIRCLE('',#3214,1.25);
#1351=CIRCLE('',#3217,1.25);
#1352=CIRCLE('',#3218,1.25);
#1353=CIRCLE('',#3236,1.);
#1354=CIRCLE('',#3237,1.);
#1355=CIRCLE('',#3239,1.);
#1356=CIRCLE('',#3240,1.);
#1357=CIRCLE('',#3253,1.);
#1358=CIRCLE('',#3254,1.);
#1359=CIRCLE('',#3256,1.);
#1360=CIRCLE('',#3257,1.);
#1361=CIRCLE('',#3270,1.);
#1362=CIRCLE('',#3271,1.);
#1363=CIRCLE('',#3273,1.);
#1364=CIRCLE('',#3274,1.);
#1365=CIRCLE('',#3287,1.);
#1366=CIRCLE('',#3288,1.);
#1367=CIRCLE('',#3290,1.);
#1368=CIRCLE('',#3291,1.);
#1369=VERTEX_POINT('',#4168);
#1370=VERTEX_POINT('',#4170);
#1371=VERTEX_POINT('',#4174);
#1372=VERTEX_POINT('',#4176);
#1373=VERTEX_POINT('',#4180);
#1374=VERTEX_POINT('',#4181);
#1375=VERTEX_POINT('',#4183);
#1376=VERTEX_POINT('',#4185);
#1377=VERTEX_POINT('',#4187);
#1378=VERTEX_POINT('',#4189);
#1379=VERTEX_POINT('',#4193);
#1380=VERTEX_POINT('',#4197);
#1381=VERTEX_POINT('',#4198);
#1382=VERTEX_POINT('',#4200);
#1383=VERTEX_POINT('',#4204);
#1384=VERTEX_POINT('',#4208);
#1385=VERTEX_POINT('',#4212);
#1386=VERTEX_POINT('',#4216);
#1387=VERTEX_POINT('',#4234);
#1388=VERTEX_POINT('',#4241);
#1389=VERTEX_POINT('',#4243);
#1390=VERTEX_POINT('',#4247);
#1391=VERTEX_POINT('',#4249);
#1392=VERTEX_POINT('',#4253);
#1393=VERTEX_POINT('',#4254);
#1394=VERTEX_POINT('',#4256);
#1395=VERTEX_POINT('',#4258);
#1396=VERTEX_POINT('',#4260);
#1397=VERTEX_POINT('',#4262);
#1398=VERTEX_POINT('',#4266);
#1399=VERTEX_POINT('',#4270);
#1400=VERTEX_POINT('',#4271);
#1401=VERTEX_POINT('',#4273);
#1402=VERTEX_POINT('',#4277);
#1403=VERTEX_POINT('',#4281);
#1404=VERTEX_POINT('',#4285);
#1405=VERTEX_POINT('',#4289);
#1406=VERTEX_POINT('',#4307);
#1407=VERTEX_POINT('',#4314);
#1408=VERTEX_POINT('',#4316);
#1409=VERTEX_POINT('',#4320);
#1410=VERTEX_POINT('',#4322);
#1411=VERTEX_POINT('',#4326);
#1412=VERTEX_POINT('',#4327);
#1413=VERTEX_POINT('',#4329);
#1414=VERTEX_POINT('',#4331);
#1415=VERTEX_POINT('',#4333);
#1416=VERTEX_POINT('',#4335);
#1417=VERTEX_POINT('',#4339);
#1418=VERTEX_POINT('',#4343);
#1419=VERTEX_POINT('',#4344);
#1420=VERTEX_POINT('',#4346);
#1421=VERTEX_POINT('',#4350);
#1422=VERTEX_POINT('',#4354);
#1423=VERTEX_POINT('',#4358);
#1424=VERTEX_POINT('',#4362);
#1425=VERTEX_POINT('',#4380);
#1426=VERTEX_POINT('',#4387);
#1427=VERTEX_POINT('',#4389);
#1428=VERTEX_POINT('',#4393);
#1429=VERTEX_POINT('',#4395);
#1430=VERTEX_POINT('',#4399);
#1431=VERTEX_POINT('',#4400);
#1432=VERTEX_POINT('',#4402);
#1433=VERTEX_POINT('',#4404);
#1434=VERTEX_POINT('',#4406);
#1435=VERTEX_POINT('',#4408);
#1436=VERTEX_POINT('',#4412);
#1437=VERTEX_POINT('',#4416);
#1438=VERTEX_POINT('',#4417);
#1439=VERTEX_POINT('',#4419);
#1440=VERTEX_POINT('',#4423);
#1441=VERTEX_POINT('',#4427);
#1442=VERTEX_POINT('',#4431);
#1443=VERTEX_POINT('',#4435);
#1444=VERTEX_POINT('',#4453);
#1445=VERTEX_POINT('',#4460);
#1446=VERTEX_POINT('',#4462);
#1447=VERTEX_POINT('',#4466);
#1448=VERTEX_POINT('',#4467);
#1449=VERTEX_POINT('',#4469);
#1450=VERTEX_POINT('',#4471);
#1451=VERTEX_POINT('',#4474);
#1452=VERTEX_POINT('',#4476);
#1453=VERTEX_POINT('',#4478);
#1454=VERTEX_POINT('',#4480);
#1455=VERTEX_POINT('',#4483);
#1456=VERTEX_POINT('',#4487);
#1457=VERTEX_POINT('',#4491);
#1458=VERTEX_POINT('',#4495);
#1459=VERTEX_POINT('',#4499);
#1460=VERTEX_POINT('',#4503);
#1461=VERTEX_POINT('',#4507);
#1462=VERTEX_POINT('',#4511);
#1463=VERTEX_POINT('',#4515);
#1464=VERTEX_POINT('',#4519);
#1465=VERTEX_POINT('',#4521);
#1466=VERTEX_POINT('',#4526);
#1467=VERTEX_POINT('',#4528);
#1468=VERTEX_POINT('',#4533);
#1469=VERTEX_POINT('',#4535);
#1470=VERTEX_POINT('',#4540);
#1471=VERTEX_POINT('',#4542);
#1472=VERTEX_POINT('',#4547);
#1473=VERTEX_POINT('',#4549);
#1474=VERTEX_POINT('',#4554);
#1475=VERTEX_POINT('',#4555);
#1476=VERTEX_POINT('',#4557);
#1477=VERTEX_POINT('',#4559);
#1478=VERTEX_POINT('',#4563);
#1479=VERTEX_POINT('',#4565);
#1480=VERTEX_POINT('',#4572);
#1481=VERTEX_POINT('',#4573);
#1482=VERTEX_POINT('',#4578);
#1483=VERTEX_POINT('',#4579);
#1484=VERTEX_POINT('',#4581);
#1485=VERTEX_POINT('',#4583);
#1486=VERTEX_POINT('',#4588);
#1487=VERTEX_POINT('',#4590);
#1488=VERTEX_POINT('',#4594);
#1489=VERTEX_POINT('',#4600);
#1490=VERTEX_POINT('',#4608);
#1491=VERTEX_POINT('',#4610);
#1492=VERTEX_POINT('',#4615);
#1493=VERTEX_POINT('',#4617);
#1494=VERTEX_POINT('',#4622);
#1495=VERTEX_POINT('',#4624);
#1496=VERTEX_POINT('',#4629);
#1497=VERTEX_POINT('',#4631);
#1498=VERTEX_POINT('',#4636);
#1499=VERTEX_POINT('',#4637);
#1500=VERTEX_POINT('',#4639);
#1501=VERTEX_POINT('',#4641);
#1502=VERTEX_POINT('',#4643);
#1503=VERTEX_POINT('',#4645);
#1504=VERTEX_POINT('',#4647);
#1505=VERTEX_POINT('',#4649);
#1506=VERTEX_POINT('',#4651);
#1507=VERTEX_POINT('',#4653);
#1508=VERTEX_POINT('',#4655);
#1509=VERTEX_POINT('',#4657);
#1510=VERTEX_POINT('',#4661);
#1511=VERTEX_POINT('',#4663);
#1512=VERTEX_POINT('',#4667);
#1513=VERTEX_POINT('',#4671);
#1514=VERTEX_POINT('',#4675);
#1515=VERTEX_POINT('',#4679);
#1516=VERTEX_POINT('',#4683);
#1517=VERTEX_POINT('',#4687);
#1518=VERTEX_POINT('',#4691);
#1519=VERTEX_POINT('',#4695);
#1520=VERTEX_POINT('',#4699);
#1521=VERTEX_POINT('',#4703);
#1522=VERTEX_POINT('',#4711);
#1523=VERTEX_POINT('',#4713);
#1524=VERTEX_POINT('',#4717);
#1525=VERTEX_POINT('',#4719);
#1526=VERTEX_POINT('',#4723);
#1527=VERTEX_POINT('',#4724);
#1528=VERTEX_POINT('',#4726);
#1529=VERTEX_POINT('',#4728);
#1530=VERTEX_POINT('',#4732);
#1531=VERTEX_POINT('',#4734);
#1532=VERTEX_POINT('',#4738);
#1533=VERTEX_POINT('',#4740);
#1534=VERTEX_POINT('',#4744);
#1535=VERTEX_POINT('',#4746);
#1536=VERTEX_POINT('',#4750);
#1537=VERTEX_POINT('',#4752);
#1538=VERTEX_POINT('',#4756);
#1539=VERTEX_POINT('',#4758);
#1540=VERTEX_POINT('',#4762);
#1541=VERTEX_POINT('',#4764);
#1542=VERTEX_POINT('',#4774);
#1543=VERTEX_POINT('',#4776);
#1544=VERTEX_POINT('',#4780);
#1545=VERTEX_POINT('',#4782);
#1546=VERTEX_POINT('',#4786);
#1547=VERTEX_POINT('',#4787);
#1548=VERTEX_POINT('',#4789);
#1549=VERTEX_POINT('',#4791);
#1550=VERTEX_POINT('',#4795);
#1551=VERTEX_POINT('',#4797);
#1552=VERTEX_POINT('',#4801);
#1553=VERTEX_POINT('',#4803);
#1554=VERTEX_POINT('',#4807);
#1555=VERTEX_POINT('',#4809);
#1556=VERTEX_POINT('',#4813);
#1557=VERTEX_POINT('',#4815);
#1558=VERTEX_POINT('',#4819);
#1559=VERTEX_POINT('',#4821);
#1560=VERTEX_POINT('',#4825);
#1561=VERTEX_POINT('',#4827);
#1562=VERTEX_POINT('',#4837);
#1563=VERTEX_POINT('',#4839);
#1564=VERTEX_POINT('',#4843);
#1565=VERTEX_POINT('',#4845);
#1566=VERTEX_POINT('',#4849);
#1567=VERTEX_POINT('',#4850);
#1568=VERTEX_POINT('',#4852);
#1569=VERTEX_POINT('',#4854);
#1570=VERTEX_POINT('',#4858);
#1571=VERTEX_POINT('',#4860);
#1572=VERTEX_POINT('',#4864);
#1573=VERTEX_POINT('',#4866);
#1574=VERTEX_POINT('',#4870);
#1575=VERTEX_POINT('',#4872);
#1576=VERTEX_POINT('',#4876);
#1577=VERTEX_POINT('',#4878);
#1578=VERTEX_POINT('',#4882);
#1579=VERTEX_POINT('',#4884);
#1580=VERTEX_POINT('',#4888);
#1581=VERTEX_POINT('',#4890);
#1582=VERTEX_POINT('',#4900);
#1583=VERTEX_POINT('',#4902);
#1584=VERTEX_POINT('',#4906);
#1585=VERTEX_POINT('',#4908);
#1586=VERTEX_POINT('',#4912);
#1587=VERTEX_POINT('',#4913);
#1588=VERTEX_POINT('',#4915);
#1589=VERTEX_POINT('',#4917);
#1590=VERTEX_POINT('',#4921);
#1591=VERTEX_POINT('',#4923);
#1592=VERTEX_POINT('',#4927);
#1593=VERTEX_POINT('',#4929);
#1594=VERTEX_POINT('',#4933);
#1595=VERTEX_POINT('',#4935);
#1596=VERTEX_POINT('',#4939);
#1597=VERTEX_POINT('',#4941);
#1598=VERTEX_POINT('',#4945);
#1599=VERTEX_POINT('',#4947);
#1600=VERTEX_POINT('',#4951);
#1601=VERTEX_POINT('',#4953);
#1602=EDGE_CURVE('',#1369,#1369,#1288,.T.);
#1603=EDGE_CURVE('',#1369,#1370,#702,.T.);
#1604=EDGE_CURVE('',#1370,#1370,#1289,.T.);
#1605=EDGE_CURVE('',#1371,#1371,#1290,.T.);
#1606=EDGE_CURVE('',#1371,#1372,#1291,.T.);
#1607=EDGE_CURVE('',#1372,#1372,#1292,.T.);
#1608=EDGE_CURVE('',#1373,#1374,#703,.T.);
#1609=EDGE_CURVE('',#1374,#1375,#704,.T.);
#1610=EDGE_CURVE('',#1375,#1376,#705,.T.);
#1611=EDGE_CURVE('',#1376,#1377,#706,.T.);
#1612=EDGE_CURVE('',#1377,#1378,#707,.T.);
#1613=EDGE_CURVE('',#1378,#1373,#708,.T.);
#1614=EDGE_CURVE('',#1379,#1379,#1293,.T.);
#1615=EDGE_CURVE('',#1379,#1371,#709,.T.);
#1616=EDGE_CURVE('',#1380,#1381,#710,.T.);
#1617=EDGE_CURVE('',#1382,#1380,#711,.T.);
#1618=EDGE_CURVE('',#1382,#1381,#712,.T.);
#1619=EDGE_CURVE('',#1383,#1382,#713,.T.);
#1620=EDGE_CURVE('',#1383,#1381,#714,.T.);
#1621=EDGE_CURVE('',#1384,#1383,#715,.T.);
#1622=EDGE_CURVE('',#1384,#1381,#716,.T.);
#1623=EDGE_CURVE('',#1385,#1384,#717,.T.);
#1624=EDGE_CURVE('',#1385,#1381,#718,.T.);
#1625=EDGE_CURVE('',#1386,#1385,#719,.T.);
#1626=EDGE_CURVE('',#1386,#1381,#720,.T.);
#1627=EDGE_CURVE('',#1380,#1386,#721,.T.);
#1628=EDGE_CURVE('',#1373,#1382,#722,.T.);
#1629=EDGE_CURVE('',#1374,#1380,#723,.T.);
#1630=EDGE_CURVE('',#1378,#1383,#724,.T.);
#1631=EDGE_CURVE('',#1377,#1384,#725,.T.);
#1632=EDGE_CURVE('',#1376,#1385,#726,.T.);
#1633=EDGE_CURVE('',#1375,#1386,#727,.T.);
#1634=EDGE_CURVE('',#1369,#1387,#728,.T.);
#1635=EDGE_CURVE('',#1387,#1387,#1294,.F.);
#1636=EDGE_CURVE('',#1388,#1388,#1295,.T.);
#1637=EDGE_CURVE('',#1388,#1389,#729,.T.);
#1638=EDGE_CURVE('',#1389,#1389,#1296,.T.);
#1639=EDGE_CURVE('',#1390,#1390,#1297,.T.);
#1640=EDGE_CURVE('',#1390,#1391,#1298,.T.);
#1641=EDGE_CURVE('',#1391,#1391,#1299,.T.);
#1642=EDGE_CURVE('',#1392,#1393,#730,.T.);
#1643=EDGE_CURVE('',#1393,#1394,#731,.T.);
#1644=EDGE_CURVE('',#1394,#1395,#732,.T.);
#1645=EDGE_CURVE('',#1395,#1396,#733,.T.);
#1646=EDGE_CURVE('',#1396,#1397,#734,.T.);
#1647=EDGE_CURVE('',#1397,#1392,#735,.T.);
#1648=EDGE_CURVE('',#1398,#1398,#1300,.T.);
#1649=EDGE_CURVE('',#1398,#1390,#736,.T.);
#1650=EDGE_CURVE('',#1399,#1400,#737,.T.);
#1651=EDGE_CURVE('',#1401,#1399,#738,.T.);
#1652=EDGE_CURVE('',#1401,#1400,#739,.T.);
#1653=EDGE_CURVE('',#1402,#1401,#740,.T.);
#1654=EDGE_CURVE('',#1402,#1400,#741,.T.);
#1655=EDGE_CURVE('',#1403,#1402,#742,.T.);
#1656=EDGE_CURVE('',#1403,#1400,#743,.T.);
#1657=EDGE_CURVE('',#1404,#1403,#744,.T.);
#1658=EDGE_CURVE('',#1404,#1400,#745,.T.);
#1659=EDGE_CURVE('',#1405,#1404,#746,.T.);
#1660=EDGE_CURVE('',#1405,#1400,#747,.T.);
#1661=EDGE_CURVE('',#1399,#1405,#748,.T.);
#1662=EDGE_CURVE('',#1392,#1401,#749,.T.);
#1663=EDGE_CURVE('',#1393,#1399,#750,.T.);
#1664=EDGE_CURVE('',#1397,#1402,#751,.T.);
#1665=EDGE_CURVE('',#1396,#1403,#752,.T.);
#1666=EDGE_CURVE('',#1395,#1404,#753,.T.);
#1667=EDGE_CURVE('',#1394,#1405,#754,.T.);
#1668=EDGE_CURVE('',#1388,#1406,#755,.T.);
#1669=EDGE_CURVE('',#1406,#1406,#1301,.F.);
#1670=EDGE_CURVE('',#1407,#1407,#1302,.T.);
#1671=EDGE_CURVE('',#1407,#1408,#756,.T.);
#1672=EDGE_CURVE('',#1408,#1408,#1303,.T.);
#1673=EDGE_CURVE('',#1409,#1409,#1304,.T.);
#1674=EDGE_CURVE('',#1409,#1410,#1305,.T.);
#1675=EDGE_CURVE('',#1410,#1410,#1306,.T.);
#1676=EDGE_CURVE('',#1411,#1412,#757,.T.);
#1677=EDGE_CURVE('',#1412,#1413,#758,.T.);
#1678=EDGE_CURVE('',#1413,#1414,#759,.T.);
#1679=EDGE_CURVE('',#1414,#1415,#760,.T.);
#1680=EDGE_CURVE('',#1415,#1416,#761,.T.);
#1681=EDGE_CURVE('',#1416,#1411,#762,.T.);
#1682=EDGE_CURVE('',#1417,#1417,#1307,.T.);
#1683=EDGE_CURVE('',#1417,#1409,#763,.T.);
#1684=EDGE_CURVE('',#1418,#1419,#764,.T.);
#1685=EDGE_CURVE('',#1420,#1418,#765,.T.);
#1686=EDGE_CURVE('',#1420,#1419,#766,.T.);
#1687=EDGE_CURVE('',#1421,#1420,#767,.T.);
#1688=EDGE_CURVE('',#1421,#1419,#768,.T.);
#1689=EDGE_CURVE('',#1422,#1421,#769,.T.);
#1690=EDGE_CURVE('',#1422,#1419,#770,.T.);
#1691=EDGE_CURVE('',#1423,#1422,#771,.T.);
#1692=EDGE_CURVE('',#1423,#1419,#772,.T.);
#1693=EDGE_CURVE('',#1424,#1423,#773,.T.);
#1694=EDGE_CURVE('',#1424,#1419,#774,.T.);
#1695=EDGE_CURVE('',#1418,#1424,#775,.T.);
#1696=EDGE_CURVE('',#1411,#1420,#776,.T.);
#1697=EDGE_CURVE('',#1412,#1418,#777,.T.);
#1698=EDGE_CURVE('',#1416,#1421,#778,.T.);
#1699=EDGE_CURVE('',#1415,#1422,#779,.T.);
#1700=EDGE_CURVE('',#1414,#1423,#780,.T.);
#1701=EDGE_CURVE('',#1413,#1424,#781,.T.);
#1702=EDGE_CURVE('',#1407,#1425,#782,.T.);
#1703=EDGE_CURVE('',#1425,#1425,#1308,.F.);
#1704=EDGE_CURVE('',#1426,#1426,#1309,.T.);
#1705=EDGE_CURVE('',#1426,#1427,#783,.T.);
#1706=EDGE_CURVE('',#1427,#1427,#1310,.T.);
#1707=EDGE_CURVE('',#1428,#1428,#1311,.T.);
#1708=EDGE_CURVE('',#1428,#1429,#1312,.T.);
#1709=EDGE_CURVE('',#1429,#1429,#1313,.T.);
#1710=EDGE_CURVE('',#1430,#1431,#784,.T.);
#1711=EDGE_CURVE('',#1431,#1432,#785,.T.);
#1712=EDGE_CURVE('',#1432,#1433,#786,.T.);
#1713=EDGE_CURVE('',#1433,#1434,#787,.T.);
#1714=EDGE_CURVE('',#1434,#1435,#788,.T.);
#1715=EDGE_CURVE('',#1435,#1430,#789,.T.);
#1716=EDGE_CURVE('',#1436,#1436,#1314,.T.);
#1717=EDGE_CURVE('',#1436,#1428,#790,.T.);
#1718=EDGE_CURVE('',#1437,#1438,#791,.T.);
#1719=EDGE_CURVE('',#1439,#1437,#792,.T.);
#1720=EDGE_CURVE('',#1439,#1438,#793,.T.);
#1721=EDGE_CURVE('',#1440,#1439,#794,.T.);
#1722=EDGE_CURVE('',#1440,#1438,#795,.T.);
#1723=EDGE_CURVE('',#1441,#1440,#796,.T.);
#1724=EDGE_CURVE('',#1441,#1438,#797,.T.);
#1725=EDGE_CURVE('',#1442,#1441,#798,.T.);
#1726=EDGE_CURVE('',#1442,#1438,#799,.T.);
#1727=EDGE_CURVE('',#1443,#1442,#800,.T.);
#1728=EDGE_CURVE('',#1443,#1438,#801,.T.);
#1729=EDGE_CURVE('',#1437,#1443,#802,.T.);
#1730=EDGE_CURVE('',#1430,#1439,#803,.T.);
#1731=EDGE_CURVE('',#1431,#1437,#804,.T.);
#1732=EDGE_CURVE('',#1435,#1440,#805,.T.);
#1733=EDGE_CURVE('',#1434,#1441,#806,.T.);
#1734=EDGE_CURVE('',#1433,#1442,#807,.T.);
#1735=EDGE_CURVE('',#1432,#1443,#808,.T.);
#1736=EDGE_CURVE('',#1426,#1444,#809,.T.);
#1737=EDGE_CURVE('',#1444,#1444,#1315,.F.);
#1738=EDGE_CURVE('',#1445,#1445,#1316,.T.);
#1739=EDGE_CURVE('',#1445,#1446,#810,.T.);
#1740=EDGE_CURVE('',#1446,#1446,#1317,.T.);
#1741=EDGE_CURVE('',#1447,#1448,#811,.T.);
#1742=EDGE_CURVE('',#1448,#1449,#812,.T.);
#1743=EDGE_CURVE('',#1450,#1449,#813,.T.);
#1744=EDGE_CURVE('',#1447,#1450,#814,.T.);
#1745=EDGE_CURVE('',#1451,#1451,#1318,.T.);
#1746=EDGE_CURVE('',#1452,#1452,#1319,.T.);
#1747=EDGE_CURVE('',#1453,#1453,#1320,.T.);
#1748=EDGE_CURVE('',#1454,#1454,#1321,.T.);
#1749=EDGE_CURVE('',#1455,#1455,#1322,.T.);
#1750=EDGE_CURVE('',#1455,#1445,#815,.T.);
#1751=EDGE_CURVE('',#1456,#1456,#1323,.T.);
#1752=EDGE_CURVE('',#1456,#1451,#816,.T.);
#1753=EDGE_CURVE('',#1457,#1457,#1324,.T.);
#1754=EDGE_CURVE('',#1457,#1456,#817,.T.);
#1755=EDGE_CURVE('',#1458,#1458,#1325,.T.);
#1756=EDGE_CURVE('',#1458,#1454,#818,.T.);
#1757=EDGE_CURVE('',#1459,#1459,#1326,.T.);
#1758=EDGE_CURVE('',#1459,#1458,#819,.T.);
#1759=EDGE_CURVE('',#1460,#1460,#1327,.T.);
#1760=EDGE_CURVE('',#1460,#1452,#820,.T.);
#1761=EDGE_CURVE('',#1461,#1461,#1328,.T.);
#1762=EDGE_CURVE('',#1461,#1460,#821,.T.);
#1763=EDGE_CURVE('',#1462,#1462,#1329,.T.);
#1764=EDGE_CURVE('',#1462,#1453,#822,.T.);
#1765=EDGE_CURVE('',#1463,#1463,#1330,.T.);
#1766=EDGE_CURVE('',#1463,#1462,#823,.T.);
#1767=EDGE_CURVE('',#1464,#1464,#1331,.T.);
#1768=EDGE_CURVE('',#1464,#1465,#824,.T.);
#1769=EDGE_CURVE('',#1465,#1465,#1332,.T.);
#1770=EDGE_CURVE('',#1466,#1466,#1333,.T.);
#1771=EDGE_CURVE('',#1466,#1467,#825,.T.);
#1772=EDGE_CURVE('',#1467,#1467,#1334,.T.);
#1773=EDGE_CURVE('',#1468,#1468,#1335,.T.);
#1774=EDGE_CURVE('',#1468,#1469,#826,.T.);
#1775=EDGE_CURVE('',#1469,#1469,#1336,.T.);
#1776=EDGE_CURVE('',#1470,#1470,#1337,.T.);
#1777=EDGE_CURVE('',#1470,#1471,#827,.T.);
#1778=EDGE_CURVE('',#1471,#1471,#1338,.T.);
#1779=EDGE_CURVE('',#1472,#1472,#1339,.T.);
#1780=EDGE_CURVE('',#1472,#1473,#828,.T.);
#1781=EDGE_CURVE('',#1473,#1473,#1340,.T.);
#1782=EDGE_CURVE('',#1474,#1475,#829,.T.);
#1783=EDGE_CURVE('',#1475,#1476,#830,.T.);
#1784=EDGE_CURVE('',#1476,#1477,#831,.T.);
#1785=EDGE_CURVE('',#1477,#1474,#832,.T.);
#1786=EDGE_CURVE('',#1476,#1478,#1341,.T.);
#1787=EDGE_CURVE('',#1478,#1479,#833,.T.);
#1788=EDGE_CURVE('',#1479,#1477,#1342,.T.);
#1789=EDGE_CURVE('',#1478,#1450,#834,.T.);
#1790=EDGE_CURVE('',#1449,#1479,#835,.T.);
#1791=EDGE_CURVE('',#1480,#1481,#836,.T.);
#1792=EDGE_CURVE('',#1480,#1475,#837,.T.);
#1793=EDGE_CURVE('',#1474,#1481,#838,.T.);
#1794=EDGE_CURVE('',#1482,#1483,#839,.T.);
#1795=EDGE_CURVE('',#1483,#1484,#840,.T.);
#1796=EDGE_CURVE('',#1484,#1485,#1343,.T.);
#1797=EDGE_CURVE('',#1485,#1447,#841,.T.);
#1798=EDGE_CURVE('',#1482,#1480,#842,.T.);
#1799=EDGE_CURVE('',#1486,#1483,#843,.T.);
#1800=EDGE_CURVE('',#1487,#1486,#844,.T.);
#1801=EDGE_CURVE('',#1484,#1487,#845,.T.);
#1802=EDGE_CURVE('',#1488,#1487,#1344,.T.);
#1803=EDGE_CURVE('',#1485,#1488,#846,.T.);
#1804=EDGE_CURVE('',#1448,#1488,#847,.T.);
#1805=EDGE_CURVE('',#1489,#1481,#848,.T.);
#1806=EDGE_CURVE('',#1482,#1489,#849,.T.);
#1807=EDGE_CURVE('',#1486,#1489,#850,.T.);
#1808=EDGE_CURVE('',#1490,#1490,#1345,.T.);
#1809=EDGE_CURVE('',#1490,#1491,#851,.T.);
#1810=EDGE_CURVE('',#1491,#1491,#1346,.T.);
#1811=EDGE_CURVE('',#1492,#1492,#1347,.T.);
#1812=EDGE_CURVE('',#1492,#1493,#852,.T.);
#1813=EDGE_CURVE('',#1493,#1493,#1348,.T.);
#1814=EDGE_CURVE('',#1494,#1494,#1349,.T.);
#1815=EDGE_CURVE('',#1494,#1495,#853,.T.);
#1816=EDGE_CURVE('',#1495,#1495,#1350,.T.);
#1817=EDGE_CURVE('',#1496,#1496,#1351,.T.);
#1818=EDGE_CURVE('',#1496,#1497,#854,.T.);
#1819=EDGE_CURVE('',#1497,#1497,#1352,.T.);
#1820=EDGE_CURVE('',#1498,#1499,#855,.T.);
#1821=EDGE_CURVE('',#1499,#1500,#856,.T.);
#1822=EDGE_CURVE('',#1500,#1501,#857,.T.);
#1823=EDGE_CURVE('',#1501,#1502,#858,.T.);
#1824=EDGE_CURVE('',#1502,#1503,#859,.T.);
#1825=EDGE_CURVE('',#1503,#1504,#860,.T.);
#1826=EDGE_CURVE('',#1504,#1505,#861,.T.);
#1827=EDGE_CURVE('',#1505,#1506,#862,.T.);
#1828=EDGE_CURVE('',#1506,#1507,#863,.T.);
#1829=EDGE_CURVE('',#1507,#1508,#864,.T.);
#1830=EDGE_CURVE('',#1508,#1509,#865,.T.);
#1831=EDGE_CURVE('',#1509,#1498,#866,.T.);
#1832=EDGE_CURVE('',#1499,#1510,#867,.T.);
#1833=EDGE_CURVE('',#1511,#1510,#868,.T.);
#1834=EDGE_CURVE('',#1500,#1511,#869,.T.);
#1835=EDGE_CURVE('',#1512,#1511,#870,.T.);
#1836=EDGE_CURVE('',#1501,#1512,#871,.T.);
#1837=EDGE_CURVE('',#1513,#1512,#872,.T.);
#1838=EDGE_CURVE('',#1502,#1513,#873,.T.);
#1839=EDGE_CURVE('',#1514,#1513,#874,.T.);
#1840=EDGE_CURVE('',#1503,#1514,#875,.T.);
#1841=EDGE_CURVE('',#1515,#1514,#876,.T.);
#1842=EDGE_CURVE('',#1504,#1515,#877,.T.);
#1843=EDGE_CURVE('',#1516,#1515,#878,.T.);
#1844=EDGE_CURVE('',#1505,#1516,#879,.T.);
#1845=EDGE_CURVE('',#1517,#1516,#880,.T.);
#1846=EDGE_CURVE('',#1506,#1517,#881,.T.);
#1847=EDGE_CURVE('',#1518,#1517,#882,.T.);
#1848=EDGE_CURVE('',#1507,#1518,#883,.T.);
#1849=EDGE_CURVE('',#1519,#1518,#884,.T.);
#1850=EDGE_CURVE('',#1508,#1519,#885,.T.);
#1851=EDGE_CURVE('',#1520,#1519,#886,.T.);
#1852=EDGE_CURVE('',#1509,#1520,#887,.T.);
#1853=EDGE_CURVE('',#1521,#1520,#888,.T.);
#1854=EDGE_CURVE('',#1498,#1521,#889,.T.);
#1855=EDGE_CURVE('',#1510,#1521,#890,.T.);
#1856=EDGE_CURVE('',#1522,#1522,#1353,.T.);
#1857=EDGE_CURVE('',#1522,#1523,#891,.T.);
#1858=EDGE_CURVE('',#1523,#1523,#1354,.T.);
#1859=EDGE_CURVE('',#1524,#1524,#1355,.T.);
#1860=EDGE_CURVE('',#1524,#1525,#892,.T.);
#1861=EDGE_CURVE('',#1525,#1525,#1356,.T.);
#1862=EDGE_CURVE('',#1526,#1527,#893,.T.);
#1863=EDGE_CURVE('',#1526,#1528,#894,.T.);
#1864=EDGE_CURVE('',#1528,#1529,#895,.T.);
#1865=EDGE_CURVE('',#1527,#1529,#896,.T.);
#1866=EDGE_CURVE('',#1530,#1526,#897,.T.);
#1867=EDGE_CURVE('',#1530,#1531,#898,.T.);
#1868=EDGE_CURVE('',#1531,#1528,#899,.T.);
#1869=EDGE_CURVE('',#1532,#1530,#900,.T.);
#1870=EDGE_CURVE('',#1532,#1533,#901,.T.);
#1871=EDGE_CURVE('',#1533,#1531,#902,.T.);
#1872=EDGE_CURVE('',#1534,#1532,#903,.T.);
#1873=EDGE_CURVE('',#1534,#1535,#904,.T.);
#1874=EDGE_CURVE('',#1535,#1533,#905,.T.);
#1875=EDGE_CURVE('',#1536,#1534,#906,.T.);
#1876=EDGE_CURVE('',#1536,#1537,#907,.T.);
#1877=EDGE_CURVE('',#1537,#1535,#908,.T.);
#1878=EDGE_CURVE('',#1538,#1536,#909,.T.);
#1879=EDGE_CURVE('',#1538,#1539,#910,.T.);
#1880=EDGE_CURVE('',#1539,#1537,#911,.T.);
#1881=EDGE_CURVE('',#1540,#1538,#912,.T.);
#1882=EDGE_CURVE('',#1540,#1541,#913,.T.);
#1883=EDGE_CURVE('',#1541,#1539,#914,.T.);
#1884=EDGE_CURVE('',#1527,#1540,#915,.T.);
#1885=EDGE_CURVE('',#1529,#1541,#916,.T.);
#1886=EDGE_CURVE('',#1542,#1542,#1357,.T.);
#1887=EDGE_CURVE('',#1542,#1543,#917,.T.);
#1888=EDGE_CURVE('',#1543,#1543,#1358,.T.);
#1889=EDGE_CURVE('',#1544,#1544,#1359,.T.);
#1890=EDGE_CURVE('',#1544,#1545,#918,.T.);
#1891=EDGE_CURVE('',#1545,#1545,#1360,.T.);
#1892=EDGE_CURVE('',#1546,#1547,#919,.T.);
#1893=EDGE_CURVE('',#1547,#1548,#920,.T.);
#1894=EDGE_CURVE('',#1549,#1548,#921,.T.);
#1895=EDGE_CURVE('',#1546,#1549,#922,.T.);
#1896=EDGE_CURVE('',#1550,#1546,#923,.T.);
#1897=EDGE_CURVE('',#1551,#1549,#924,.T.);
#1898=EDGE_CURVE('',#1550,#1551,#925,.T.);
#1899=EDGE_CURVE('',#1552,#1550,#926,.T.);
#1900=EDGE_CURVE('',#1553,#1551,#927,.T.);
#1901=EDGE_CURVE('',#1552,#1553,#928,.T.);
#1902=EDGE_CURVE('',#1554,#1552,#929,.T.);
#1903=EDGE_CURVE('',#1555,#1553,#930,.T.);
#1904=EDGE_CURVE('',#1554,#1555,#931,.T.);
#1905=EDGE_CURVE('',#1556,#1554,#932,.T.);
#1906=EDGE_CURVE('',#1557,#1555,#933,.T.);
#1907=EDGE_CURVE('',#1556,#1557,#934,.T.);
#1908=EDGE_CURVE('',#1558,#1556,#935,.T.);
#1909=EDGE_CURVE('',#1559,#1557,#936,.T.);
#1910=EDGE_CURVE('',#1558,#1559,#937,.T.);
#1911=EDGE_CURVE('',#1560,#1558,#938,.T.);
#1912=EDGE_CURVE('',#1561,#1559,#939,.T.);
#1913=EDGE_CURVE('',#1560,#1561,#940,.T.);
#1914=EDGE_CURVE('',#1547,#1560,#941,.T.);
#1915=EDGE_CURVE('',#1548,#1561,#942,.T.);
#1916=EDGE_CURVE('',#1562,#1562,#1361,.T.);
#1917=EDGE_CURVE('',#1562,#1563,#943,.T.);
#1918=EDGE_CURVE('',#1563,#1563,#1362,.T.);
#1919=EDGE_CURVE('',#1564,#1564,#1363,.T.);
#1920=EDGE_CURVE('',#1564,#1565,#944,.T.);
#1921=EDGE_CURVE('',#1565,#1565,#1364,.T.);
#1922=EDGE_CURVE('',#1566,#1567,#945,.T.);
#1923=EDGE_CURVE('',#1566,#1568,#946,.T.);
#1924=EDGE_CURVE('',#1568,#1569,#947,.T.);
#1925=EDGE_CURVE('',#1567,#1569,#948,.T.);
#1926=EDGE_CURVE('',#1570,#1566,#949,.T.);
#1927=EDGE_CURVE('',#1570,#1571,#950,.T.);
#1928=EDGE_CURVE('',#1571,#1568,#951,.T.);
#1929=EDGE_CURVE('',#1572,#1570,#952,.T.);
#1930=EDGE_CURVE('',#1572,#1573,#953,.T.);
#1931=EDGE_CURVE('',#1573,#1571,#954,.T.);
#1932=EDGE_CURVE('',#1574,#1572,#955,.T.);
#1933=EDGE_CURVE('',#1574,#1575,#956,.T.);
#1934=EDGE_CURVE('',#1575,#1573,#957,.T.);
#1935=EDGE_CURVE('',#1576,#1574,#958,.T.);
#1936=EDGE_CURVE('',#1576,#1577,#959,.T.);
#1937=EDGE_CURVE('',#1577,#1575,#960,.T.);
#1938=EDGE_CURVE('',#1578,#1576,#961,.T.);
#1939=EDGE_CURVE('',#1578,#1579,#962,.T.);
#1940=EDGE_CURVE('',#1579,#1577,#963,.T.);
#1941=EDGE_CURVE('',#1580,#1578,#964,.T.);
#1942=EDGE_CURVE('',#1580,#1581,#965,.T.);
#1943=EDGE_CURVE('',#1581,#1579,#966,.T.);
#1944=EDGE_CURVE('',#1567,#1580,#967,.T.);
#1945=EDGE_CURVE('',#1569,#1581,#968,.T.);
#1946=EDGE_CURVE('',#1582,#1582,#1365,.T.);
#1947=EDGE_CURVE('',#1582,#1583,#969,.T.);
#1948=EDGE_CURVE('',#1583,#1583,#1366,.T.);
#1949=EDGE_CURVE('',#1584,#1584,#1367,.T.);
#1950=EDGE_CURVE('',#1584,#1585,#970,.T.);
#1951=EDGE_CURVE('',#1585,#1585,#1368,.T.);
#1952=EDGE_CURVE('',#1586,#1587,#971,.T.);
#1953=EDGE_CURVE('',#1587,#1588,#972,.T.);
#1954=EDGE_CURVE('',#1589,#1588,#973,.T.);
#1955=EDGE_CURVE('',#1586,#1589,#974,.T.);
#1956=EDGE_CURVE('',#1590,#1586,#975,.T.);
#1957=EDGE_CURVE('',#1591,#1589,#976,.T.);
#1958=EDGE_CURVE('',#1590,#1591,#977,.T.);
#1959=EDGE_CURVE('',#1592,#1590,#978,.T.);
#1960=EDGE_CURVE('',#1593,#1591,#979,.T.);
#1961=EDGE_CURVE('',#1592,#1593,#980,.T.);
#1962=EDGE_CURVE('',#1594,#1592,#981,.T.);
#1963=EDGE_CURVE('',#1595,#1593,#982,.T.);
#1964=EDGE_CURVE('',#1594,#1595,#983,.T.);
#1965=EDGE_CURVE('',#1596,#1594,#984,.T.);
#1966=EDGE_CURVE('',#1597,#1595,#985,.T.);
#1967=EDGE_CURVE('',#1596,#1597,#986,.T.);
#1968=EDGE_CURVE('',#1598,#1596,#987,.T.);
#1969=EDGE_CURVE('',#1599,#1597,#988,.T.);
#1970=EDGE_CURVE('',#1598,#1599,#989,.T.);
#1971=EDGE_CURVE('',#1600,#1598,#990,.T.);
#1972=EDGE_CURVE('',#1601,#1599,#991,.T.);
#1973=EDGE_CURVE('',#1600,#1601,#992,.T.);
#1974=EDGE_CURVE('',#1587,#1600,#993,.T.);
#1975=EDGE_CURVE('',#1588,#1601,#994,.T.);
#1976=ORIENTED_EDGE('',*,*,#1602,.F.);
#1977=ORIENTED_EDGE('',*,*,#1603,.T.);
#1978=ORIENTED_EDGE('',*,*,#1604,.F.);
#1979=ORIENTED_EDGE('',*,*,#1603,.F.);
#1980=ORIENTED_EDGE('',*,*,#1605,.T.);
#1981=ORIENTED_EDGE('',*,*,#1606,.T.);
#1982=ORIENTED_EDGE('',*,*,#1607,.T.);
#1983=ORIENTED_EDGE('',*,*,#1606,.F.);
#1984=ORIENTED_EDGE('',*,*,#1607,.F.);
#1985=ORIENTED_EDGE('',*,*,#1608,.T.);
#1986=ORIENTED_EDGE('',*,*,#1609,.T.);
#1987=ORIENTED_EDGE('',*,*,#1610,.T.);
#1988=ORIENTED_EDGE('',*,*,#1611,.T.);
#1989=ORIENTED_EDGE('',*,*,#1612,.T.);
#1990=ORIENTED_EDGE('',*,*,#1613,.T.);
#1991=ORIENTED_EDGE('',*,*,#1614,.F.);
#1992=ORIENTED_EDGE('',*,*,#1615,.T.);
#1993=ORIENTED_EDGE('',*,*,#1605,.F.);
#1994=ORIENTED_EDGE('',*,*,#1615,.F.);
#1995=ORIENTED_EDGE('',*,*,#1616,.F.);
#1996=ORIENTED_EDGE('',*,*,#1617,.F.);
#1997=ORIENTED_EDGE('',*,*,#1618,.T.);
#1998=ORIENTED_EDGE('',*,*,#1618,.F.);
#1999=ORIENTED_EDGE('',*,*,#1619,.F.);
#2000=ORIENTED_EDGE('',*,*,#1620,.T.);
#2001=ORIENTED_EDGE('',*,*,#1620,.F.);
#2002=ORIENTED_EDGE('',*,*,#1621,.F.);
#2003=ORIENTED_EDGE('',*,*,#1622,.T.);
#2004=ORIENTED_EDGE('',*,*,#1622,.F.);
#2005=ORIENTED_EDGE('',*,*,#1623,.F.);
#2006=ORIENTED_EDGE('',*,*,#1624,.T.);
#2007=ORIENTED_EDGE('',*,*,#1624,.F.);
#2008=ORIENTED_EDGE('',*,*,#1625,.F.);
#2009=ORIENTED_EDGE('',*,*,#1626,.T.);
#2010=ORIENTED_EDGE('',*,*,#1626,.F.);
#2011=ORIENTED_EDGE('',*,*,#1627,.F.);
#2012=ORIENTED_EDGE('',*,*,#1616,.T.);
#2013=ORIENTED_EDGE('',*,*,#1608,.F.);
#2014=ORIENTED_EDGE('',*,*,#1628,.T.);
#2015=ORIENTED_EDGE('',*,*,#1617,.T.);
#2016=ORIENTED_EDGE('',*,*,#1629,.F.);
#2017=ORIENTED_EDGE('',*,*,#1613,.F.);
#2018=ORIENTED_EDGE('',*,*,#1630,.T.);
#2019=ORIENTED_EDGE('',*,*,#1619,.T.);
#2020=ORIENTED_EDGE('',*,*,#1628,.F.);
#2021=ORIENTED_EDGE('',*,*,#1612,.F.);
#2022=ORIENTED_EDGE('',*,*,#1631,.T.);
#2023=ORIENTED_EDGE('',*,*,#1621,.T.);
#2024=ORIENTED_EDGE('',*,*,#1630,.F.);
#2025=ORIENTED_EDGE('',*,*,#1611,.F.);
#2026=ORIENTED_EDGE('',*,*,#1632,.T.);
#2027=ORIENTED_EDGE('',*,*,#1623,.T.);
#2028=ORIENTED_EDGE('',*,*,#1631,.F.);
#2029=ORIENTED_EDGE('',*,*,#1610,.F.);
#2030=ORIENTED_EDGE('',*,*,#1633,.T.);
#2031=ORIENTED_EDGE('',*,*,#1625,.T.);
#2032=ORIENTED_EDGE('',*,*,#1632,.F.);
#2033=ORIENTED_EDGE('',*,*,#1609,.F.);
#2034=ORIENTED_EDGE('',*,*,#1629,.T.);
#2035=ORIENTED_EDGE('',*,*,#1627,.T.);
#2036=ORIENTED_EDGE('',*,*,#1633,.F.);
#2037=ORIENTED_EDGE('',*,*,#1602,.T.);
#2038=ORIENTED_EDGE('',*,*,#1634,.T.);
#2039=ORIENTED_EDGE('',*,*,#1635,.T.);
#2040=ORIENTED_EDGE('',*,*,#1634,.F.);
#2041=ORIENTED_EDGE('',*,*,#1604,.T.);
#2042=ORIENTED_EDGE('',*,*,#1614,.T.);
#2043=ORIENTED_EDGE('',*,*,#1635,.F.);
#2044=ORIENTED_EDGE('',*,*,#1636,.F.);
#2045=ORIENTED_EDGE('',*,*,#1637,.T.);
#2046=ORIENTED_EDGE('',*,*,#1638,.F.);
#2047=ORIENTED_EDGE('',*,*,#1637,.F.);
#2048=ORIENTED_EDGE('',*,*,#1639,.T.);
#2049=ORIENTED_EDGE('',*,*,#1640,.T.);
#2050=ORIENTED_EDGE('',*,*,#1641,.T.);
#2051=ORIENTED_EDGE('',*,*,#1640,.F.);
#2052=ORIENTED_EDGE('',*,*,#1641,.F.);
#2053=ORIENTED_EDGE('',*,*,#1642,.T.);
#2054=ORIENTED_EDGE('',*,*,#1643,.T.);
#2055=ORIENTED_EDGE('',*,*,#1644,.T.);
#2056=ORIENTED_EDGE('',*,*,#1645,.T.);
#2057=ORIENTED_EDGE('',*,*,#1646,.T.);
#2058=ORIENTED_EDGE('',*,*,#1647,.T.);
#2059=ORIENTED_EDGE('',*,*,#1648,.F.);
#2060=ORIENTED_EDGE('',*,*,#1649,.T.);
#2061=ORIENTED_EDGE('',*,*,#1639,.F.);
#2062=ORIENTED_EDGE('',*,*,#1649,.F.);
#2063=ORIENTED_EDGE('',*,*,#1650,.F.);
#2064=ORIENTED_EDGE('',*,*,#1651,.F.);
#2065=ORIENTED_EDGE('',*,*,#1652,.T.);
#2066=ORIENTED_EDGE('',*,*,#1652,.F.);
#2067=ORIENTED_EDGE('',*,*,#1653,.F.);
#2068=ORIENTED_EDGE('',*,*,#1654,.T.);
#2069=ORIENTED_EDGE('',*,*,#1654,.F.);
#2070=ORIENTED_EDGE('',*,*,#1655,.F.);
#2071=ORIENTED_EDGE('',*,*,#1656,.T.);
#2072=ORIENTED_EDGE('',*,*,#1656,.F.);
#2073=ORIENTED_EDGE('',*,*,#1657,.F.);
#2074=ORIENTED_EDGE('',*,*,#1658,.T.);
#2075=ORIENTED_EDGE('',*,*,#1658,.F.);
#2076=ORIENTED_EDGE('',*,*,#1659,.F.);
#2077=ORIENTED_EDGE('',*,*,#1660,.T.);
#2078=ORIENTED_EDGE('',*,*,#1660,.F.);
#2079=ORIENTED_EDGE('',*,*,#1661,.F.);
#2080=ORIENTED_EDGE('',*,*,#1650,.T.);
#2081=ORIENTED_EDGE('',*,*,#1642,.F.);
#2082=ORIENTED_EDGE('',*,*,#1662,.T.);
#2083=ORIENTED_EDGE('',*,*,#1651,.T.);
#2084=ORIENTED_EDGE('',*,*,#1663,.F.);
#2085=ORIENTED_EDGE('',*,*,#1647,.F.);
#2086=ORIENTED_EDGE('',*,*,#1664,.T.);
#2087=ORIENTED_EDGE('',*,*,#1653,.T.);
#2088=ORIENTED_EDGE('',*,*,#1662,.F.);
#2089=ORIENTED_EDGE('',*,*,#1646,.F.);
#2090=ORIENTED_EDGE('',*,*,#1665,.T.);
#2091=ORIENTED_EDGE('',*,*,#1655,.T.);
#2092=ORIENTED_EDGE('',*,*,#1664,.F.);
#2093=ORIENTED_EDGE('',*,*,#1645,.F.);
#2094=ORIENTED_EDGE('',*,*,#1666,.T.);
#2095=ORIENTED_EDGE('',*,*,#1657,.T.);
#2096=ORIENTED_EDGE('',*,*,#1665,.F.);
#2097=ORIENTED_EDGE('',*,*,#1644,.F.);
#2098=ORIENTED_EDGE('',*,*,#1667,.T.);
#2099=ORIENTED_EDGE('',*,*,#1659,.T.);
#2100=ORIENTED_EDGE('',*,*,#1666,.F.);
#2101=ORIENTED_EDGE('',*,*,#1643,.F.);
#2102=ORIENTED_EDGE('',*,*,#1663,.T.);
#2103=ORIENTED_EDGE('',*,*,#1661,.T.);
#2104=ORIENTED_EDGE('',*,*,#1667,.F.);
#2105=ORIENTED_EDGE('',*,*,#1636,.T.);
#2106=ORIENTED_EDGE('',*,*,#1668,.T.);
#2107=ORIENTED_EDGE('',*,*,#1669,.T.);
#2108=ORIENTED_EDGE('',*,*,#1668,.F.);
#2109=ORIENTED_EDGE('',*,*,#1638,.T.);
#2110=ORIENTED_EDGE('',*,*,#1648,.T.);
#2111=ORIENTED_EDGE('',*,*,#1669,.F.);
#2112=ORIENTED_EDGE('',*,*,#1670,.F.);
#2113=ORIENTED_EDGE('',*,*,#1671,.T.);
#2114=ORIENTED_EDGE('',*,*,#1672,.F.);
#2115=ORIENTED_EDGE('',*,*,#1671,.F.);
#2116=ORIENTED_EDGE('',*,*,#1673,.T.);
#2117=ORIENTED_EDGE('',*,*,#1674,.T.);
#2118=ORIENTED_EDGE('',*,*,#1675,.T.);
#2119=ORIENTED_EDGE('',*,*,#1674,.F.);
#2120=ORIENTED_EDGE('',*,*,#1675,.F.);
#2121=ORIENTED_EDGE('',*,*,#1676,.T.);
#2122=ORIENTED_EDGE('',*,*,#1677,.T.);
#2123=ORIENTED_EDGE('',*,*,#1678,.T.);
#2124=ORIENTED_EDGE('',*,*,#1679,.T.);
#2125=ORIENTED_EDGE('',*,*,#1680,.T.);
#2126=ORIENTED_EDGE('',*,*,#1681,.T.);
#2127=ORIENTED_EDGE('',*,*,#1682,.F.);
#2128=ORIENTED_EDGE('',*,*,#1683,.T.);
#2129=ORIENTED_EDGE('',*,*,#1673,.F.);
#2130=ORIENTED_EDGE('',*,*,#1683,.F.);
#2131=ORIENTED_EDGE('',*,*,#1684,.F.);
#2132=ORIENTED_EDGE('',*,*,#1685,.F.);
#2133=ORIENTED_EDGE('',*,*,#1686,.T.);
#2134=ORIENTED_EDGE('',*,*,#1686,.F.);
#2135=ORIENTED_EDGE('',*,*,#1687,.F.);
#2136=ORIENTED_EDGE('',*,*,#1688,.T.);
#2137=ORIENTED_EDGE('',*,*,#1688,.F.);
#2138=ORIENTED_EDGE('',*,*,#1689,.F.);
#2139=ORIENTED_EDGE('',*,*,#1690,.T.);
#2140=ORIENTED_EDGE('',*,*,#1690,.F.);
#2141=ORIENTED_EDGE('',*,*,#1691,.F.);
#2142=ORIENTED_EDGE('',*,*,#1692,.T.);
#2143=ORIENTED_EDGE('',*,*,#1692,.F.);
#2144=ORIENTED_EDGE('',*,*,#1693,.F.);
#2145=ORIENTED_EDGE('',*,*,#1694,.T.);
#2146=ORIENTED_EDGE('',*,*,#1694,.F.);
#2147=ORIENTED_EDGE('',*,*,#1695,.F.);
#2148=ORIENTED_EDGE('',*,*,#1684,.T.);
#2149=ORIENTED_EDGE('',*,*,#1676,.F.);
#2150=ORIENTED_EDGE('',*,*,#1696,.T.);
#2151=ORIENTED_EDGE('',*,*,#1685,.T.);
#2152=ORIENTED_EDGE('',*,*,#1697,.F.);
#2153=ORIENTED_EDGE('',*,*,#1681,.F.);
#2154=ORIENTED_EDGE('',*,*,#1698,.T.);
#2155=ORIENTED_EDGE('',*,*,#1687,.T.);
#2156=ORIENTED_EDGE('',*,*,#1696,.F.);
#2157=ORIENTED_EDGE('',*,*,#1680,.F.);
#2158=ORIENTED_EDGE('',*,*,#1699,.T.);
#2159=ORIENTED_EDGE('',*,*,#1689,.T.);
#2160=ORIENTED_EDGE('',*,*,#1698,.F.);
#2161=ORIENTED_EDGE('',*,*,#1679,.F.);
#2162=ORIENTED_EDGE('',*,*,#1700,.T.);
#2163=ORIENTED_EDGE('',*,*,#1691,.T.);
#2164=ORIENTED_EDGE('',*,*,#1699,.F.);
#2165=ORIENTED_EDGE('',*,*,#1678,.F.);
#2166=ORIENTED_EDGE('',*,*,#1701,.T.);
#2167=ORIENTED_EDGE('',*,*,#1693,.T.);
#2168=ORIENTED_EDGE('',*,*,#1700,.F.);
#2169=ORIENTED_EDGE('',*,*,#1677,.F.);
#2170=ORIENTED_EDGE('',*,*,#1697,.T.);
#2171=ORIENTED_EDGE('',*,*,#1695,.T.);
#2172=ORIENTED_EDGE('',*,*,#1701,.F.);
#2173=ORIENTED_EDGE('',*,*,#1670,.T.);
#2174=ORIENTED_EDGE('',*,*,#1702,.T.);
#2175=ORIENTED_EDGE('',*,*,#1703,.T.);
#2176=ORIENTED_EDGE('',*,*,#1702,.F.);
#2177=ORIENTED_EDGE('',*,*,#1672,.T.);
#2178=ORIENTED_EDGE('',*,*,#1682,.T.);
#2179=ORIENTED_EDGE('',*,*,#1703,.F.);
#2180=ORIENTED_EDGE('',*,*,#1704,.F.);
#2181=ORIENTED_EDGE('',*,*,#1705,.T.);
#2182=ORIENTED_EDGE('',*,*,#1706,.F.);
#2183=ORIENTED_EDGE('',*,*,#1705,.F.);
#2184=ORIENTED_EDGE('',*,*,#1707,.T.);
#2185=ORIENTED_EDGE('',*,*,#1708,.T.);
#2186=ORIENTED_EDGE('',*,*,#1709,.T.);
#2187=ORIENTED_EDGE('',*,*,#1708,.F.);
#2188=ORIENTED_EDGE('',*,*,#1709,.F.);
#2189=ORIENTED_EDGE('',*,*,#1710,.T.);
#2190=ORIENTED_EDGE('',*,*,#1711,.T.);
#2191=ORIENTED_EDGE('',*,*,#1712,.T.);
#2192=ORIENTED_EDGE('',*,*,#1713,.T.);
#2193=ORIENTED_EDGE('',*,*,#1714,.T.);
#2194=ORIENTED_EDGE('',*,*,#1715,.T.);
#2195=ORIENTED_EDGE('',*,*,#1716,.F.);
#2196=ORIENTED_EDGE('',*,*,#1717,.T.);
#2197=ORIENTED_EDGE('',*,*,#1707,.F.);
#2198=ORIENTED_EDGE('',*,*,#1717,.F.);
#2199=ORIENTED_EDGE('',*,*,#1718,.F.);
#2200=ORIENTED_EDGE('',*,*,#1719,.F.);
#2201=ORIENTED_EDGE('',*,*,#1720,.T.);
#2202=ORIENTED_EDGE('',*,*,#1720,.F.);
#2203=ORIENTED_EDGE('',*,*,#1721,.F.);
#2204=ORIENTED_EDGE('',*,*,#1722,.T.);
#2205=ORIENTED_EDGE('',*,*,#1722,.F.);
#2206=ORIENTED_EDGE('',*,*,#1723,.F.);
#2207=ORIENTED_EDGE('',*,*,#1724,.T.);
#2208=ORIENTED_EDGE('',*,*,#1724,.F.);
#2209=ORIENTED_EDGE('',*,*,#1725,.F.);
#2210=ORIENTED_EDGE('',*,*,#1726,.T.);
#2211=ORIENTED_EDGE('',*,*,#1726,.F.);
#2212=ORIENTED_EDGE('',*,*,#1727,.F.);
#2213=ORIENTED_EDGE('',*,*,#1728,.T.);
#2214=ORIENTED_EDGE('',*,*,#1728,.F.);
#2215=ORIENTED_EDGE('',*,*,#1729,.F.);
#2216=ORIENTED_EDGE('',*,*,#1718,.T.);
#2217=ORIENTED_EDGE('',*,*,#1710,.F.);
#2218=ORIENTED_EDGE('',*,*,#1730,.T.);
#2219=ORIENTED_EDGE('',*,*,#1719,.T.);
#2220=ORIENTED_EDGE('',*,*,#1731,.F.);
#2221=ORIENTED_EDGE('',*,*,#1715,.F.);
#2222=ORIENTED_EDGE('',*,*,#1732,.T.);
#2223=ORIENTED_EDGE('',*,*,#1721,.T.);
#2224=ORIENTED_EDGE('',*,*,#1730,.F.);
#2225=ORIENTED_EDGE('',*,*,#1714,.F.);
#2226=ORIENTED_EDGE('',*,*,#1733,.T.);
#2227=ORIENTED_EDGE('',*,*,#1723,.T.);
#2228=ORIENTED_EDGE('',*,*,#1732,.F.);
#2229=ORIENTED_EDGE('',*,*,#1713,.F.);
#2230=ORIENTED_EDGE('',*,*,#1734,.T.);
#2231=ORIENTED_EDGE('',*,*,#1725,.T.);
#2232=ORIENTED_EDGE('',*,*,#1733,.F.);
#2233=ORIENTED_EDGE('',*,*,#1712,.F.);
#2234=ORIENTED_EDGE('',*,*,#1735,.T.);
#2235=ORIENTED_EDGE('',*,*,#1727,.T.);
#2236=ORIENTED_EDGE('',*,*,#1734,.F.);
#2237=ORIENTED_EDGE('',*,*,#1711,.F.);
#2238=ORIENTED_EDGE('',*,*,#1731,.T.);
#2239=ORIENTED_EDGE('',*,*,#1729,.T.);
#2240=ORIENTED_EDGE('',*,*,#1735,.F.);
#2241=ORIENTED_EDGE('',*,*,#1704,.T.);
#2242=ORIENTED_EDGE('',*,*,#1736,.T.);
#2243=ORIENTED_EDGE('',*,*,#1737,.T.);
#2244=ORIENTED_EDGE('',*,*,#1736,.F.);
#2245=ORIENTED_EDGE('',*,*,#1706,.T.);
#2246=ORIENTED_EDGE('',*,*,#1716,.T.);
#2247=ORIENTED_EDGE('',*,*,#1737,.F.);
#2248=ORIENTED_EDGE('',*,*,#1738,.T.);
#2249=ORIENTED_EDGE('',*,*,#1739,.T.);
#2250=ORIENTED_EDGE('',*,*,#1740,.T.);
#2251=ORIENTED_EDGE('',*,*,#1739,.F.);
#2252=ORIENTED_EDGE('',*,*,#1741,.T.);
#2253=ORIENTED_EDGE('',*,*,#1742,.T.);
#2254=ORIENTED_EDGE('',*,*,#1743,.F.);
#2255=ORIENTED_EDGE('',*,*,#1744,.F.);
#2256=ORIENTED_EDGE('',*,*,#1745,.F.);
#2257=ORIENTED_EDGE('',*,*,#1746,.F.);
#2258=ORIENTED_EDGE('',*,*,#1747,.F.);
#2259=ORIENTED_EDGE('',*,*,#1748,.F.);
#2260=ORIENTED_EDGE('',*,*,#1740,.F.);
#2261=ORIENTED_EDGE('',*,*,#1749,.T.);
#2262=ORIENTED_EDGE('',*,*,#1750,.T.);
#2263=ORIENTED_EDGE('',*,*,#1738,.F.);
#2264=ORIENTED_EDGE('',*,*,#1750,.F.);
#2265=ORIENTED_EDGE('',*,*,#1751,.T.);
#2266=ORIENTED_EDGE('',*,*,#1752,.T.);
#2267=ORIENTED_EDGE('',*,*,#1745,.T.);
#2268=ORIENTED_EDGE('',*,*,#1752,.F.);
#2269=ORIENTED_EDGE('',*,*,#1753,.T.);
#2270=ORIENTED_EDGE('',*,*,#1754,.T.);
#2271=ORIENTED_EDGE('',*,*,#1751,.F.);
#2272=ORIENTED_EDGE('',*,*,#1754,.F.);
#2273=ORIENTED_EDGE('',*,*,#1755,.T.);
#2274=ORIENTED_EDGE('',*,*,#1756,.T.);
#2275=ORIENTED_EDGE('',*,*,#1748,.T.);
#2276=ORIENTED_EDGE('',*,*,#1756,.F.);
#2277=ORIENTED_EDGE('',*,*,#1757,.T.);
#2278=ORIENTED_EDGE('',*,*,#1758,.T.);
#2279=ORIENTED_EDGE('',*,*,#1755,.F.);
#2280=ORIENTED_EDGE('',*,*,#1758,.F.);
#2281=ORIENTED_EDGE('',*,*,#1759,.T.);
#2282=ORIENTED_EDGE('',*,*,#1760,.T.);
#2283=ORIENTED_EDGE('',*,*,#1746,.T.);
#2284=ORIENTED_EDGE('',*,*,#1760,.F.);
#2285=ORIENTED_EDGE('',*,*,#1761,.T.);
#2286=ORIENTED_EDGE('',*,*,#1762,.T.);
#2287=ORIENTED_EDGE('',*,*,#1759,.F.);
#2288=ORIENTED_EDGE('',*,*,#1762,.F.);
#2289=ORIENTED_EDGE('',*,*,#1763,.T.);
#2290=ORIENTED_EDGE('',*,*,#1764,.T.);
#2291=ORIENTED_EDGE('',*,*,#1747,.T.);
#2292=ORIENTED_EDGE('',*,*,#1764,.F.);
#2293=ORIENTED_EDGE('',*,*,#1765,.T.);
#2294=ORIENTED_EDGE('',*,*,#1766,.T.);
#2295=ORIENTED_EDGE('',*,*,#1763,.F.);
#2296=ORIENTED_EDGE('',*,*,#1766,.F.);
#2297=ORIENTED_EDGE('',*,*,#1767,.F.);
#2298=ORIENTED_EDGE('',*,*,#1768,.T.);
#2299=ORIENTED_EDGE('',*,*,#1769,.T.);
#2300=ORIENTED_EDGE('',*,*,#1768,.F.);
#2301=ORIENTED_EDGE('',*,*,#1769,.F.);
#2302=ORIENTED_EDGE('',*,*,#1757,.F.);
#2303=ORIENTED_EDGE('',*,*,#1770,.F.);
#2304=ORIENTED_EDGE('',*,*,#1771,.T.);
#2305=ORIENTED_EDGE('',*,*,#1772,.T.);
#2306=ORIENTED_EDGE('',*,*,#1771,.F.);
#2307=ORIENTED_EDGE('',*,*,#1772,.F.);
#2308=ORIENTED_EDGE('',*,*,#1761,.F.);
#2309=ORIENTED_EDGE('',*,*,#1773,.F.);
#2310=ORIENTED_EDGE('',*,*,#1774,.T.);
#2311=ORIENTED_EDGE('',*,*,#1775,.T.);
#2312=ORIENTED_EDGE('',*,*,#1774,.F.);
#2313=ORIENTED_EDGE('',*,*,#1775,.F.);
#2314=ORIENTED_EDGE('',*,*,#1753,.F.);
#2315=ORIENTED_EDGE('',*,*,#1776,.F.);
#2316=ORIENTED_EDGE('',*,*,#1777,.T.);
#2317=ORIENTED_EDGE('',*,*,#1778,.T.);
#2318=ORIENTED_EDGE('',*,*,#1777,.F.);
#2319=ORIENTED_EDGE('',*,*,#1778,.F.);
#2320=ORIENTED_EDGE('',*,*,#1765,.F.);
#2321=ORIENTED_EDGE('',*,*,#1779,.F.);
#2322=ORIENTED_EDGE('',*,*,#1780,.T.);
#2323=ORIENTED_EDGE('',*,*,#1781,.T.);
#2324=ORIENTED_EDGE('',*,*,#1780,.F.);
#2325=ORIENTED_EDGE('',*,*,#1781,.F.);
#2326=ORIENTED_EDGE('',*,*,#1749,.F.);
#2327=ORIENTED_EDGE('',*,*,#1782,.T.);
#2328=ORIENTED_EDGE('',*,*,#1783,.T.);
#2329=ORIENTED_EDGE('',*,*,#1784,.T.);
#2330=ORIENTED_EDGE('',*,*,#1785,.T.);
#2331=ORIENTED_EDGE('',*,*,#1784,.F.);
#2332=ORIENTED_EDGE('',*,*,#1786,.T.);
#2333=ORIENTED_EDGE('',*,*,#1787,.T.);
#2334=ORIENTED_EDGE('',*,*,#1788,.T.);
#2335=ORIENTED_EDGE('',*,*,#1787,.F.);
#2336=ORIENTED_EDGE('',*,*,#1789,.T.);
#2337=ORIENTED_EDGE('',*,*,#1743,.T.);
#2338=ORIENTED_EDGE('',*,*,#1790,.T.);
#2339=ORIENTED_EDGE('',*,*,#1791,.F.);
#2340=ORIENTED_EDGE('',*,*,#1792,.T.);
#2341=ORIENTED_EDGE('',*,*,#1782,.F.);
#2342=ORIENTED_EDGE('',*,*,#1793,.T.);
#2343=ORIENTED_EDGE('',*,*,#1794,.T.);
#2344=ORIENTED_EDGE('',*,*,#1795,.T.);
#2345=ORIENTED_EDGE('',*,*,#1796,.T.);
#2346=ORIENTED_EDGE('',*,*,#1797,.T.);
#2347=ORIENTED_EDGE('',*,*,#1744,.T.);
#2348=ORIENTED_EDGE('',*,*,#1789,.F.);
#2349=ORIENTED_EDGE('',*,*,#1786,.F.);
#2350=ORIENTED_EDGE('',*,*,#1783,.F.);
#2351=ORIENTED_EDGE('',*,*,#1792,.F.);
#2352=ORIENTED_EDGE('',*,*,#1798,.F.);
#2353=ORIENTED_EDGE('',*,*,#1799,.F.);
#2354=ORIENTED_EDGE('',*,*,#1800,.F.);
#2355=ORIENTED_EDGE('',*,*,#1801,.F.);
#2356=ORIENTED_EDGE('',*,*,#1795,.F.);
#2357=ORIENTED_EDGE('',*,*,#1801,.T.);
#2358=ORIENTED_EDGE('',*,*,#1802,.F.);
#2359=ORIENTED_EDGE('',*,*,#1803,.F.);
#2360=ORIENTED_EDGE('',*,*,#1796,.F.);
#2361=ORIENTED_EDGE('',*,*,#1803,.T.);
#2362=ORIENTED_EDGE('',*,*,#1804,.F.);
#2363=ORIENTED_EDGE('',*,*,#1741,.F.);
#2364=ORIENTED_EDGE('',*,*,#1797,.F.);
#2365=ORIENTED_EDGE('',*,*,#1805,.F.);
#2366=ORIENTED_EDGE('',*,*,#1806,.F.);
#2367=ORIENTED_EDGE('',*,*,#1798,.T.);
#2368=ORIENTED_EDGE('',*,*,#1791,.T.);
#2369=ORIENTED_EDGE('',*,*,#1779,.T.);
#2370=ORIENTED_EDGE('',*,*,#1776,.T.);
#2371=ORIENTED_EDGE('',*,*,#1773,.T.);
#2372=ORIENTED_EDGE('',*,*,#1770,.T.);
#2373=ORIENTED_EDGE('',*,*,#1767,.T.);
#2374=ORIENTED_EDGE('',*,*,#1806,.T.);
#2375=ORIENTED_EDGE('',*,*,#1807,.F.);
#2376=ORIENTED_EDGE('',*,*,#1799,.T.);
#2377=ORIENTED_EDGE('',*,*,#1794,.F.);
#2378=ORIENTED_EDGE('',*,*,#1807,.T.);
#2379=ORIENTED_EDGE('',*,*,#1805,.T.);
#2380=ORIENTED_EDGE('',*,*,#1793,.F.);
#2381=ORIENTED_EDGE('',*,*,#1785,.F.);
#2382=ORIENTED_EDGE('',*,*,#1788,.F.);
#2383=ORIENTED_EDGE('',*,*,#1790,.F.);
#2384=ORIENTED_EDGE('',*,*,#1742,.F.);
#2385=ORIENTED_EDGE('',*,*,#1804,.T.);
#2386=ORIENTED_EDGE('',*,*,#1802,.T.);
#2387=ORIENTED_EDGE('',*,*,#1800,.T.);
#2388=ORIENTED_EDGE('',*,*,#1808,.F.);
#2389=ORIENTED_EDGE('',*,*,#1809,.T.);
#2390=ORIENTED_EDGE('',*,*,#1810,.T.);
#2391=ORIENTED_EDGE('',*,*,#1809,.F.);
#2392=ORIENTED_EDGE('',*,*,#1810,.F.);
#2393=ORIENTED_EDGE('',*,*,#1811,.F.);
#2394=ORIENTED_EDGE('',*,*,#1812,.T.);
#2395=ORIENTED_EDGE('',*,*,#1813,.T.);
#2396=ORIENTED_EDGE('',*,*,#1812,.F.);
#2397=ORIENTED_EDGE('',*,*,#1813,.F.);
#2398=ORIENTED_EDGE('',*,*,#1814,.F.);
#2399=ORIENTED_EDGE('',*,*,#1815,.T.);
#2400=ORIENTED_EDGE('',*,*,#1816,.T.);
#2401=ORIENTED_EDGE('',*,*,#1815,.F.);
#2402=ORIENTED_EDGE('',*,*,#1816,.F.);
#2403=ORIENTED_EDGE('',*,*,#1817,.F.);
#2404=ORIENTED_EDGE('',*,*,#1818,.T.);
#2405=ORIENTED_EDGE('',*,*,#1819,.T.);
#2406=ORIENTED_EDGE('',*,*,#1818,.F.);
#2407=ORIENTED_EDGE('',*,*,#1819,.F.);
#2408=ORIENTED_EDGE('',*,*,#1820,.T.);
#2409=ORIENTED_EDGE('',*,*,#1821,.T.);
#2410=ORIENTED_EDGE('',*,*,#1822,.T.);
#2411=ORIENTED_EDGE('',*,*,#1823,.T.);
#2412=ORIENTED_EDGE('',*,*,#1824,.T.);
#2413=ORIENTED_EDGE('',*,*,#1825,.T.);
#2414=ORIENTED_EDGE('',*,*,#1826,.T.);
#2415=ORIENTED_EDGE('',*,*,#1827,.T.);
#2416=ORIENTED_EDGE('',*,*,#1828,.T.);
#2417=ORIENTED_EDGE('',*,*,#1829,.T.);
#2418=ORIENTED_EDGE('',*,*,#1830,.T.);
#2419=ORIENTED_EDGE('',*,*,#1831,.T.);
#2420=ORIENTED_EDGE('',*,*,#1832,.T.);
#2421=ORIENTED_EDGE('',*,*,#1833,.F.);
#2422=ORIENTED_EDGE('',*,*,#1834,.F.);
#2423=ORIENTED_EDGE('',*,*,#1821,.F.);
#2424=ORIENTED_EDGE('',*,*,#1834,.T.);
#2425=ORIENTED_EDGE('',*,*,#1835,.F.);
#2426=ORIENTED_EDGE('',*,*,#1836,.F.);
#2427=ORIENTED_EDGE('',*,*,#1822,.F.);
#2428=ORIENTED_EDGE('',*,*,#1836,.T.);
#2429=ORIENTED_EDGE('',*,*,#1837,.F.);
#2430=ORIENTED_EDGE('',*,*,#1838,.F.);
#2431=ORIENTED_EDGE('',*,*,#1823,.F.);
#2432=ORIENTED_EDGE('',*,*,#1838,.T.);
#2433=ORIENTED_EDGE('',*,*,#1839,.F.);
#2434=ORIENTED_EDGE('',*,*,#1840,.F.);
#2435=ORIENTED_EDGE('',*,*,#1824,.F.);
#2436=ORIENTED_EDGE('',*,*,#1808,.T.);
#2437=ORIENTED_EDGE('',*,*,#1814,.T.);
#2438=ORIENTED_EDGE('',*,*,#1840,.T.);
#2439=ORIENTED_EDGE('',*,*,#1841,.F.);
#2440=ORIENTED_EDGE('',*,*,#1842,.F.);
#2441=ORIENTED_EDGE('',*,*,#1825,.F.);
#2442=ORIENTED_EDGE('',*,*,#1842,.T.);
#2443=ORIENTED_EDGE('',*,*,#1843,.F.);
#2444=ORIENTED_EDGE('',*,*,#1844,.F.);
#2445=ORIENTED_EDGE('',*,*,#1826,.F.);
#2446=ORIENTED_EDGE('',*,*,#1844,.T.);
#2447=ORIENTED_EDGE('',*,*,#1845,.F.);
#2448=ORIENTED_EDGE('',*,*,#1846,.F.);
#2449=ORIENTED_EDGE('',*,*,#1827,.F.);
#2450=ORIENTED_EDGE('',*,*,#1846,.T.);
#2451=ORIENTED_EDGE('',*,*,#1847,.F.);
#2452=ORIENTED_EDGE('',*,*,#1848,.F.);
#2453=ORIENTED_EDGE('',*,*,#1828,.F.);
#2454=ORIENTED_EDGE('',*,*,#1811,.T.);
#2455=ORIENTED_EDGE('',*,*,#1817,.T.);
#2456=ORIENTED_EDGE('',*,*,#1848,.T.);
#2457=ORIENTED_EDGE('',*,*,#1849,.F.);
#2458=ORIENTED_EDGE('',*,*,#1850,.F.);
#2459=ORIENTED_EDGE('',*,*,#1829,.F.);
#2460=ORIENTED_EDGE('',*,*,#1850,.T.);
#2461=ORIENTED_EDGE('',*,*,#1851,.F.);
#2462=ORIENTED_EDGE('',*,*,#1852,.F.);
#2463=ORIENTED_EDGE('',*,*,#1830,.F.);
#2464=ORIENTED_EDGE('',*,*,#1852,.T.);
#2465=ORIENTED_EDGE('',*,*,#1853,.F.);
#2466=ORIENTED_EDGE('',*,*,#1854,.F.);
#2467=ORIENTED_EDGE('',*,*,#1831,.F.);
#2468=ORIENTED_EDGE('',*,*,#1854,.T.);
#2469=ORIENTED_EDGE('',*,*,#1855,.F.);
#2470=ORIENTED_EDGE('',*,*,#1832,.F.);
#2471=ORIENTED_EDGE('',*,*,#1820,.F.);
#2472=ORIENTED_EDGE('',*,*,#1855,.T.);
#2473=ORIENTED_EDGE('',*,*,#1853,.T.);
#2474=ORIENTED_EDGE('',*,*,#1851,.T.);
#2475=ORIENTED_EDGE('',*,*,#1849,.T.);
#2476=ORIENTED_EDGE('',*,*,#1847,.T.);
#2477=ORIENTED_EDGE('',*,*,#1845,.T.);
#2478=ORIENTED_EDGE('',*,*,#1843,.T.);
#2479=ORIENTED_EDGE('',*,*,#1841,.T.);
#2480=ORIENTED_EDGE('',*,*,#1839,.T.);
#2481=ORIENTED_EDGE('',*,*,#1837,.T.);
#2482=ORIENTED_EDGE('',*,*,#1835,.T.);
#2483=ORIENTED_EDGE('',*,*,#1833,.T.);
#2484=ORIENTED_EDGE('',*,*,#1856,.T.);
#2485=ORIENTED_EDGE('',*,*,#1857,.T.);
#2486=ORIENTED_EDGE('',*,*,#1858,.T.);
#2487=ORIENTED_EDGE('',*,*,#1857,.F.);
#2488=ORIENTED_EDGE('',*,*,#1859,.T.);
#2489=ORIENTED_EDGE('',*,*,#1860,.T.);
#2490=ORIENTED_EDGE('',*,*,#1861,.T.);
#2491=ORIENTED_EDGE('',*,*,#1860,.F.);
#2492=ORIENTED_EDGE('',*,*,#1862,.F.);
#2493=ORIENTED_EDGE('',*,*,#1863,.T.);
#2494=ORIENTED_EDGE('',*,*,#1864,.T.);
#2495=ORIENTED_EDGE('',*,*,#1865,.F.);
#2496=ORIENTED_EDGE('',*,*,#1866,.F.);
#2497=ORIENTED_EDGE('',*,*,#1867,.T.);
#2498=ORIENTED_EDGE('',*,*,#1868,.T.);
#2499=ORIENTED_EDGE('',*,*,#1863,.F.);
#2500=ORIENTED_EDGE('',*,*,#1869,.F.);
#2501=ORIENTED_EDGE('',*,*,#1870,.T.);
#2502=ORIENTED_EDGE('',*,*,#1871,.T.);
#2503=ORIENTED_EDGE('',*,*,#1867,.F.);
#2504=ORIENTED_EDGE('',*,*,#1872,.F.);
#2505=ORIENTED_EDGE('',*,*,#1873,.T.);
#2506=ORIENTED_EDGE('',*,*,#1874,.T.);
#2507=ORIENTED_EDGE('',*,*,#1870,.F.);
#2508=ORIENTED_EDGE('',*,*,#1875,.F.);
#2509=ORIENTED_EDGE('',*,*,#1876,.T.);
#2510=ORIENTED_EDGE('',*,*,#1877,.T.);
#2511=ORIENTED_EDGE('',*,*,#1873,.F.);
#2512=ORIENTED_EDGE('',*,*,#1878,.F.);
#2513=ORIENTED_EDGE('',*,*,#1879,.T.);
#2514=ORIENTED_EDGE('',*,*,#1880,.T.);
#2515=ORIENTED_EDGE('',*,*,#1876,.F.);
#2516=ORIENTED_EDGE('',*,*,#1881,.F.);
#2517=ORIENTED_EDGE('',*,*,#1882,.T.);
#2518=ORIENTED_EDGE('',*,*,#1883,.T.);
#2519=ORIENTED_EDGE('',*,*,#1879,.F.);
#2520=ORIENTED_EDGE('',*,*,#1884,.F.);
#2521=ORIENTED_EDGE('',*,*,#1865,.T.);
#2522=ORIENTED_EDGE('',*,*,#1885,.T.);
#2523=ORIENTED_EDGE('',*,*,#1882,.F.);
#2524=ORIENTED_EDGE('',*,*,#1885,.F.);
#2525=ORIENTED_EDGE('',*,*,#1864,.F.);
#2526=ORIENTED_EDGE('',*,*,#1868,.F.);
#2527=ORIENTED_EDGE('',*,*,#1871,.F.);
#2528=ORIENTED_EDGE('',*,*,#1874,.F.);
#2529=ORIENTED_EDGE('',*,*,#1877,.F.);
#2530=ORIENTED_EDGE('',*,*,#1880,.F.);
#2531=ORIENTED_EDGE('',*,*,#1883,.F.);
#2532=ORIENTED_EDGE('',*,*,#1858,.F.);
#2533=ORIENTED_EDGE('',*,*,#1861,.F.);
#2534=ORIENTED_EDGE('',*,*,#1884,.T.);
#2535=ORIENTED_EDGE('',*,*,#1881,.T.);
#2536=ORIENTED_EDGE('',*,*,#1878,.T.);
#2537=ORIENTED_EDGE('',*,*,#1875,.T.);
#2538=ORIENTED_EDGE('',*,*,#1872,.T.);
#2539=ORIENTED_EDGE('',*,*,#1869,.T.);
#2540=ORIENTED_EDGE('',*,*,#1866,.T.);
#2541=ORIENTED_EDGE('',*,*,#1862,.T.);
#2542=ORIENTED_EDGE('',*,*,#1856,.F.);
#2543=ORIENTED_EDGE('',*,*,#1859,.F.);
#2544=ORIENTED_EDGE('',*,*,#1886,.F.);
#2545=ORIENTED_EDGE('',*,*,#1887,.T.);
#2546=ORIENTED_EDGE('',*,*,#1888,.F.);
#2547=ORIENTED_EDGE('',*,*,#1887,.F.);
#2548=ORIENTED_EDGE('',*,*,#1889,.F.);
#2549=ORIENTED_EDGE('',*,*,#1890,.T.);
#2550=ORIENTED_EDGE('',*,*,#1891,.F.);
#2551=ORIENTED_EDGE('',*,*,#1890,.F.);
#2552=ORIENTED_EDGE('',*,*,#1892,.T.);
#2553=ORIENTED_EDGE('',*,*,#1893,.T.);
#2554=ORIENTED_EDGE('',*,*,#1894,.F.);
#2555=ORIENTED_EDGE('',*,*,#1895,.F.);
#2556=ORIENTED_EDGE('',*,*,#1896,.T.);
#2557=ORIENTED_EDGE('',*,*,#1895,.T.);
#2558=ORIENTED_EDGE('',*,*,#1897,.F.);
#2559=ORIENTED_EDGE('',*,*,#1898,.F.);
#2560=ORIENTED_EDGE('',*,*,#1899,.T.);
#2561=ORIENTED_EDGE('',*,*,#1898,.T.);
#2562=ORIENTED_EDGE('',*,*,#1900,.F.);
#2563=ORIENTED_EDGE('',*,*,#1901,.F.);
#2564=ORIENTED_EDGE('',*,*,#1902,.T.);
#2565=ORIENTED_EDGE('',*,*,#1901,.T.);
#2566=ORIENTED_EDGE('',*,*,#1903,.F.);
#2567=ORIENTED_EDGE('',*,*,#1904,.F.);
#2568=ORIENTED_EDGE('',*,*,#1905,.T.);
#2569=ORIENTED_EDGE('',*,*,#1904,.T.);
#2570=ORIENTED_EDGE('',*,*,#1906,.F.);
#2571=ORIENTED_EDGE('',*,*,#1907,.F.);
#2572=ORIENTED_EDGE('',*,*,#1908,.T.);
#2573=ORIENTED_EDGE('',*,*,#1907,.T.);
#2574=ORIENTED_EDGE('',*,*,#1909,.F.);
#2575=ORIENTED_EDGE('',*,*,#1910,.F.);
#2576=ORIENTED_EDGE('',*,*,#1911,.T.);
#2577=ORIENTED_EDGE('',*,*,#1910,.T.);
#2578=ORIENTED_EDGE('',*,*,#1912,.F.);
#2579=ORIENTED_EDGE('',*,*,#1913,.F.);
#2580=ORIENTED_EDGE('',*,*,#1914,.T.);
#2581=ORIENTED_EDGE('',*,*,#1913,.T.);
#2582=ORIENTED_EDGE('',*,*,#1915,.F.);
#2583=ORIENTED_EDGE('',*,*,#1893,.F.);
#2584=ORIENTED_EDGE('',*,*,#1915,.T.);
#2585=ORIENTED_EDGE('',*,*,#1912,.T.);
#2586=ORIENTED_EDGE('',*,*,#1909,.T.);
#2587=ORIENTED_EDGE('',*,*,#1906,.T.);
#2588=ORIENTED_EDGE('',*,*,#1903,.T.);
#2589=ORIENTED_EDGE('',*,*,#1900,.T.);
#2590=ORIENTED_EDGE('',*,*,#1897,.T.);
#2591=ORIENTED_EDGE('',*,*,#1894,.T.);
#2592=ORIENTED_EDGE('',*,*,#1886,.T.);
#2593=ORIENTED_EDGE('',*,*,#1889,.T.);
#2594=ORIENTED_EDGE('',*,*,#1914,.F.);
#2595=ORIENTED_EDGE('',*,*,#1892,.F.);
#2596=ORIENTED_EDGE('',*,*,#1896,.F.);
#2597=ORIENTED_EDGE('',*,*,#1899,.F.);
#2598=ORIENTED_EDGE('',*,*,#1902,.F.);
#2599=ORIENTED_EDGE('',*,*,#1905,.F.);
#2600=ORIENTED_EDGE('',*,*,#1908,.F.);
#2601=ORIENTED_EDGE('',*,*,#1911,.F.);
#2602=ORIENTED_EDGE('',*,*,#1888,.T.);
#2603=ORIENTED_EDGE('',*,*,#1891,.T.);
#2604=ORIENTED_EDGE('',*,*,#1916,.T.);
#2605=ORIENTED_EDGE('',*,*,#1917,.T.);
#2606=ORIENTED_EDGE('',*,*,#1918,.T.);
#2607=ORIENTED_EDGE('',*,*,#1917,.F.);
#2608=ORIENTED_EDGE('',*,*,#1919,.T.);
#2609=ORIENTED_EDGE('',*,*,#1920,.T.);
#2610=ORIENTED_EDGE('',*,*,#1921,.T.);
#2611=ORIENTED_EDGE('',*,*,#1920,.F.);
#2612=ORIENTED_EDGE('',*,*,#1922,.F.);
#2613=ORIENTED_EDGE('',*,*,#1923,.T.);
#2614=ORIENTED_EDGE('',*,*,#1924,.T.);
#2615=ORIENTED_EDGE('',*,*,#1925,.F.);
#2616=ORIENTED_EDGE('',*,*,#1926,.F.);
#2617=ORIENTED_EDGE('',*,*,#1927,.T.);
#2618=ORIENTED_EDGE('',*,*,#1928,.T.);
#2619=ORIENTED_EDGE('',*,*,#1923,.F.);
#2620=ORIENTED_EDGE('',*,*,#1929,.F.);
#2621=ORIENTED_EDGE('',*,*,#1930,.T.);
#2622=ORIENTED_EDGE('',*,*,#1931,.T.);
#2623=ORIENTED_EDGE('',*,*,#1927,.F.);
#2624=ORIENTED_EDGE('',*,*,#1932,.F.);
#2625=ORIENTED_EDGE('',*,*,#1933,.T.);
#2626=ORIENTED_EDGE('',*,*,#1934,.T.);
#2627=ORIENTED_EDGE('',*,*,#1930,.F.);
#2628=ORIENTED_EDGE('',*,*,#1935,.F.);
#2629=ORIENTED_EDGE('',*,*,#1936,.T.);
#2630=ORIENTED_EDGE('',*,*,#1937,.T.);
#2631=ORIENTED_EDGE('',*,*,#1933,.F.);
#2632=ORIENTED_EDGE('',*,*,#1938,.F.);
#2633=ORIENTED_EDGE('',*,*,#1939,.T.);
#2634=ORIENTED_EDGE('',*,*,#1940,.T.);
#2635=ORIENTED_EDGE('',*,*,#1936,.F.);
#2636=ORIENTED_EDGE('',*,*,#1941,.F.);
#2637=ORIENTED_EDGE('',*,*,#1942,.T.);
#2638=ORIENTED_EDGE('',*,*,#1943,.T.);
#2639=ORIENTED_EDGE('',*,*,#1939,.F.);
#2640=ORIENTED_EDGE('',*,*,#1944,.F.);
#2641=ORIENTED_EDGE('',*,*,#1925,.T.);
#2642=ORIENTED_EDGE('',*,*,#1945,.T.);
#2643=ORIENTED_EDGE('',*,*,#1942,.F.);
#2644=ORIENTED_EDGE('',*,*,#1945,.F.);
#2645=ORIENTED_EDGE('',*,*,#1924,.F.);
#2646=ORIENTED_EDGE('',*,*,#1928,.F.);
#2647=ORIENTED_EDGE('',*,*,#1931,.F.);
#2648=ORIENTED_EDGE('',*,*,#1934,.F.);
#2649=ORIENTED_EDGE('',*,*,#1937,.F.);
#2650=ORIENTED_EDGE('',*,*,#1940,.F.);
#2651=ORIENTED_EDGE('',*,*,#1943,.F.);
#2652=ORIENTED_EDGE('',*,*,#1918,.F.);
#2653=ORIENTED_EDGE('',*,*,#1921,.F.);
#2654=ORIENTED_EDGE('',*,*,#1944,.T.);
#2655=ORIENTED_EDGE('',*,*,#1941,.T.);
#2656=ORIENTED_EDGE('',*,*,#1938,.T.);
#2657=ORIENTED_EDGE('',*,*,#1935,.T.);
#2658=ORIENTED_EDGE('',*,*,#1932,.T.);
#2659=ORIENTED_EDGE('',*,*,#1929,.T.);
#2660=ORIENTED_EDGE('',*,*,#1926,.T.);
#2661=ORIENTED_EDGE('',*,*,#1922,.T.);
#2662=ORIENTED_EDGE('',*,*,#1916,.F.);
#2663=ORIENTED_EDGE('',*,*,#1919,.F.);
#2664=ORIENTED_EDGE('',*,*,#1946,.F.);
#2665=ORIENTED_EDGE('',*,*,#1947,.T.);
#2666=ORIENTED_EDGE('',*,*,#1948,.F.);
#2667=ORIENTED_EDGE('',*,*,#1947,.F.);
#2668=ORIENTED_EDGE('',*,*,#1949,.F.);
#2669=ORIENTED_EDGE('',*,*,#1950,.T.);
#2670=ORIENTED_EDGE('',*,*,#1951,.F.);
#2671=ORIENTED_EDGE('',*,*,#1950,.F.);
#2672=ORIENTED_EDGE('',*,*,#1952,.T.);
#2673=ORIENTED_EDGE('',*,*,#1953,.T.);
#2674=ORIENTED_EDGE('',*,*,#1954,.F.);
#2675=ORIENTED_EDGE('',*,*,#1955,.F.);
#2676=ORIENTED_EDGE('',*,*,#1956,.T.);
#2677=ORIENTED_EDGE('',*,*,#1955,.T.);
#2678=ORIENTED_EDGE('',*,*,#1957,.F.);
#2679=ORIENTED_EDGE('',*,*,#1958,.F.);
#2680=ORIENTED_EDGE('',*,*,#1959,.T.);
#2681=ORIENTED_EDGE('',*,*,#1958,.T.);
#2682=ORIENTED_EDGE('',*,*,#1960,.F.);
#2683=ORIENTED_EDGE('',*,*,#1961,.F.);
#2684=ORIENTED_EDGE('',*,*,#1962,.T.);
#2685=ORIENTED_EDGE('',*,*,#1961,.T.);
#2686=ORIENTED_EDGE('',*,*,#1963,.F.);
#2687=ORIENTED_EDGE('',*,*,#1964,.F.);
#2688=ORIENTED_EDGE('',*,*,#1965,.T.);
#2689=ORIENTED_EDGE('',*,*,#1964,.T.);
#2690=ORIENTED_EDGE('',*,*,#1966,.F.);
#2691=ORIENTED_EDGE('',*,*,#1967,.F.);
#2692=ORIENTED_EDGE('',*,*,#1968,.T.);
#2693=ORIENTED_EDGE('',*,*,#1967,.T.);
#2694=ORIENTED_EDGE('',*,*,#1969,.F.);
#2695=ORIENTED_EDGE('',*,*,#1970,.F.);
#2696=ORIENTED_EDGE('',*,*,#1971,.T.);
#2697=ORIENTED_EDGE('',*,*,#1970,.T.);
#2698=ORIENTED_EDGE('',*,*,#1972,.F.);
#2699=ORIENTED_EDGE('',*,*,#1973,.F.);
#2700=ORIENTED_EDGE('',*,*,#1974,.T.);
#2701=ORIENTED_EDGE('',*,*,#1973,.T.);
#2702=ORIENTED_EDGE('',*,*,#1975,.F.);
#2703=ORIENTED_EDGE('',*,*,#1953,.F.);
#2704=ORIENTED_EDGE('',*,*,#1975,.T.);
#2705=ORIENTED_EDGE('',*,*,#1972,.T.);
#2706=ORIENTED_EDGE('',*,*,#1969,.T.);
#2707=ORIENTED_EDGE('',*,*,#1966,.T.);
#2708=ORIENTED_EDGE('',*,*,#1963,.T.);
#2709=ORIENTED_EDGE('',*,*,#1960,.T.);
#2710=ORIENTED_EDGE('',*,*,#1957,.T.);
#2711=ORIENTED_EDGE('',*,*,#1954,.T.);
#2712=ORIENTED_EDGE('',*,*,#1946,.T.);
#2713=ORIENTED_EDGE('',*,*,#1949,.T.);
#2714=ORIENTED_EDGE('',*,*,#1974,.F.);
#2715=ORIENTED_EDGE('',*,*,#1952,.F.);
#2716=ORIENTED_EDGE('',*,*,#1956,.F.);
#2717=ORIENTED_EDGE('',*,*,#1959,.F.);
#2718=ORIENTED_EDGE('',*,*,#1962,.F.);
#2719=ORIENTED_EDGE('',*,*,#1965,.F.);
#2720=ORIENTED_EDGE('',*,*,#1968,.F.);
#2721=ORIENTED_EDGE('',*,*,#1971,.F.);
#2722=ORIENTED_EDGE('',*,*,#1948,.T.);
#2723=ORIENTED_EDGE('',*,*,#1951,.T.);
#2724=CONICAL_SURFACE('',#3034,0.887310000000001,0.824535502685815);
#2725=CONICAL_SURFACE('',#3061,0.887310000000001,0.824535502685815);
#2726=CONICAL_SURFACE('',#3088,0.887310000000001,0.824535502685815);
#2727=CONICAL_SURFACE('',#3115,0.887310000000001,0.824535502685815);
#2728=CONICAL_SURFACE('',#3142,1.75,0.785398163397447);
#2729=CONICAL_SURFACE('',#3152,1.75,0.785398163397447);
#2730=CONICAL_SURFACE('',#3156,1.75,0.785398163397449);
#2731=CONICAL_SURFACE('',#3160,1.75,0.78539816339745);
#2732=CONICAL_SURFACE('',#3164,1.75,0.785398163397447);
#2733=ADVANCED_FACE('',(#303),#2724,.T.);
#2734=ADVANCED_FACE('',(#304),#299,.T.);
#2735=ADVANCED_FACE('',(#305,#123),#166,.T.);
#2736=ADVANCED_FACE('',(#306),#91,.T.);
#2737=ADVANCED_FACE('',(#307),#167,.F.);
#2738=ADVANCED_FACE('',(#308),#168,.F.);
#2739=ADVANCED_FACE('',(#309),#169,.F.);
#2740=ADVANCED_FACE('',(#310),#170,.F.);
#2741=ADVANCED_FACE('',(#311),#171,.F.);
#2742=ADVANCED_FACE('',(#312),#172,.F.);
#2743=ADVANCED_FACE('',(#313),#173,.F.);
#2744=ADVANCED_FACE('',(#314),#174,.F.);
#2745=ADVANCED_FACE('',(#315),#175,.F.);
#2746=ADVANCED_FACE('',(#316),#176,.F.);
#2747=ADVANCED_FACE('',(#317),#177,.F.);
#2748=ADVANCED_FACE('',(#318),#178,.F.);
#2749=ADVANCED_FACE('',(#319),#92,.T.);
#2750=ADVANCED_FACE('',(#320),#179,.T.);
#2751=ADVANCED_FACE('',(#321,#124),#180,.T.);
#2752=ADVANCED_FACE('',(#322),#2725,.T.);
#2753=ADVANCED_FACE('',(#323),#300,.T.);
#2754=ADVANCED_FACE('',(#324,#125),#181,.T.);
#2755=ADVANCED_FACE('',(#325),#93,.T.);
#2756=ADVANCED_FACE('',(#326),#182,.F.);
#2757=ADVANCED_FACE('',(#327),#183,.F.);
#2758=ADVANCED_FACE('',(#328),#184,.F.);
#2759=ADVANCED_FACE('',(#329),#185,.F.);
#2760=ADVANCED_FACE('',(#330),#186,.F.);
#2761=ADVANCED_FACE('',(#331),#187,.F.);
#2762=ADVANCED_FACE('',(#332),#188,.F.);
#2763=ADVANCED_FACE('',(#333),#189,.F.);
#2764=ADVANCED_FACE('',(#334),#190,.F.);
#2765=ADVANCED_FACE('',(#335),#191,.F.);
#2766=ADVANCED_FACE('',(#336),#192,.F.);
#2767=ADVANCED_FACE('',(#337),#193,.F.);
#2768=ADVANCED_FACE('',(#338),#94,.T.);
#2769=ADVANCED_FACE('',(#339),#194,.T.);
#2770=ADVANCED_FACE('',(#340,#126),#195,.T.);
#2771=ADVANCED_FACE('',(#341),#2726,.T.);
#2772=ADVANCED_FACE('',(#342),#301,.T.);
#2773=ADVANCED_FACE('',(#343,#127),#196,.T.);
#2774=ADVANCED_FACE('',(#344),#95,.T.);
#2775=ADVANCED_FACE('',(#345),#197,.F.);
#2776=ADVANCED_FACE('',(#346),#198,.F.);
#2777=ADVANCED_FACE('',(#347),#199,.F.);
#2778=ADVANCED_FACE('',(#348),#200,.F.);
#2779=ADVANCED_FACE('',(#349),#201,.F.);
#2780=ADVANCED_FACE('',(#350),#202,.F.);
#2781=ADVANCED_FACE('',(#351),#203,.F.);
#2782=ADVANCED_FACE('',(#352),#204,.F.);
#2783=ADVANCED_FACE('',(#353),#205,.F.);
#2784=ADVANCED_FACE('',(#354),#206,.F.);
#2785=ADVANCED_FACE('',(#355),#207,.F.);
#2786=ADVANCED_FACE('',(#356),#208,.F.);
#2787=ADVANCED_FACE('',(#357),#96,.T.);
#2788=ADVANCED_FACE('',(#358),#209,.T.);
#2789=ADVANCED_FACE('',(#359,#128),#210,.T.);
#2790=ADVANCED_FACE('',(#360),#2727,.T.);
#2791=ADVANCED_FACE('',(#361),#302,.T.);
#2792=ADVANCED_FACE('',(#362,#129),#211,.T.);
#2793=ADVANCED_FACE('',(#363),#97,.T.);
#2794=ADVANCED_FACE('',(#364),#212,.F.);
#2795=ADVANCED_FACE('',(#365),#213,.F.);
#2796=ADVANCED_FACE('',(#366),#214,.F.);
#2797=ADVANCED_FACE('',(#367),#215,.F.);
#2798=ADVANCED_FACE('',(#368),#216,.F.);
#2799=ADVANCED_FACE('',(#369),#217,.F.);
#2800=ADVANCED_FACE('',(#370),#218,.F.);
#2801=ADVANCED_FACE('',(#371),#219,.F.);
#2802=ADVANCED_FACE('',(#372),#220,.F.);
#2803=ADVANCED_FACE('',(#373),#221,.F.);
#2804=ADVANCED_FACE('',(#374),#222,.F.);
#2805=ADVANCED_FACE('',(#375),#223,.F.);
#2806=ADVANCED_FACE('',(#376),#98,.T.);
#2807=ADVANCED_FACE('',(#377),#224,.T.);
#2808=ADVANCED_FACE('',(#378,#130),#225,.T.);
#2809=ADVANCED_FACE('',(#379),#2728,.F.);
#2810=ADVANCED_FACE('',(#380,#131,#132,#133,#134,#135),#226,.T.);
#2811=ADVANCED_FACE('',(#381),#99,.F.);
#2812=ADVANCED_FACE('',(#382),#2729,.F.);
#2813=ADVANCED_FACE('',(#383),#100,.F.);
#2814=ADVANCED_FACE('',(#384),#2730,.F.);
#2815=ADVANCED_FACE('',(#385),#101,.F.);
#2816=ADVANCED_FACE('',(#386),#2731,.F.);
#2817=ADVANCED_FACE('',(#387),#102,.F.);
#2818=ADVANCED_FACE('',(#388),#2732,.F.);
#2819=ADVANCED_FACE('',(#389),#103,.F.);
#2820=ADVANCED_FACE('',(#390),#104,.F.);
#2821=ADVANCED_FACE('',(#391,#136),#227,.T.);
#2822=ADVANCED_FACE('',(#392),#105,.F.);
#2823=ADVANCED_FACE('',(#393,#137),#228,.T.);
#2824=ADVANCED_FACE('',(#394),#106,.F.);
#2825=ADVANCED_FACE('',(#395,#138),#229,.T.);
#2826=ADVANCED_FACE('',(#396),#107,.F.);
#2827=ADVANCED_FACE('',(#397,#139),#230,.T.);
#2828=ADVANCED_FACE('',(#398),#108,.F.);
#2829=ADVANCED_FACE('',(#399,#140),#231,.T.);
#2830=ADVANCED_FACE('',(#400),#232,.F.);
#2831=ADVANCED_FACE('',(#401),#109,.F.);
#2832=ADVANCED_FACE('',(#402),#233,.F.);
#2833=ADVANCED_FACE('',(#403),#234,.F.);
#2834=ADVANCED_FACE('',(#404),#235,.F.);
#2835=ADVANCED_FACE('',(#405),#236,.T.);
#2836=ADVANCED_FACE('',(#406),#110,.F.);
#2837=ADVANCED_FACE('',(#407),#237,.T.);
#2838=ADVANCED_FACE('',(#408,#141,#142,#143,#144,#145),#238,.T.);
#2839=ADVANCED_FACE('',(#409),#239,.T.);
#2840=ADVANCED_FACE('',(#410),#240,.T.);
#2841=ADVANCED_FACE('',(#411),#111,.F.);
#2842=ADVANCED_FACE('',(#412),#241,.T.);
#2843=ADVANCED_FACE('',(#413),#112,.F.);
#2844=ADVANCED_FACE('',(#414),#242,.T.);
#2845=ADVANCED_FACE('',(#415),#113,.F.);
#2846=ADVANCED_FACE('',(#416),#243,.T.);
#2847=ADVANCED_FACE('',(#417),#114,.F.);
#2848=ADVANCED_FACE('',(#418),#244,.T.);
#2849=ADVANCED_FACE('',(#419),#245,.T.);
#2850=ADVANCED_FACE('',(#420),#246,.T.);
#2851=ADVANCED_FACE('',(#421),#247,.T.);
#2852=ADVANCED_FACE('',(#422),#248,.T.);
#2853=ADVANCED_FACE('',(#423,#146,#147),#249,.T.);
#2854=ADVANCED_FACE('',(#424),#250,.T.);
#2855=ADVANCED_FACE('',(#425),#251,.T.);
#2856=ADVANCED_FACE('',(#426),#252,.T.);
#2857=ADVANCED_FACE('',(#427,#148,#149),#253,.T.);
#2858=ADVANCED_FACE('',(#428),#254,.T.);
#2859=ADVANCED_FACE('',(#429),#255,.T.);
#2860=ADVANCED_FACE('',(#430),#256,.T.);
#2861=ADVANCED_FACE('',(#431),#257,.T.);
#2862=ADVANCED_FACE('',(#432),#258,.T.);
#2863=ADVANCED_FACE('',(#433),#115,.F.);
#2864=ADVANCED_FACE('',(#434),#116,.F.);
#2865=ADVANCED_FACE('',(#435),#259,.F.);
#2866=ADVANCED_FACE('',(#436),#260,.F.);
#2867=ADVANCED_FACE('',(#437),#261,.F.);
#2868=ADVANCED_FACE('',(#438),#262,.F.);
#2869=ADVANCED_FACE('',(#439),#263,.F.);
#2870=ADVANCED_FACE('',(#440),#264,.F.);
#2871=ADVANCED_FACE('',(#441),#265,.F.);
#2872=ADVANCED_FACE('',(#442),#266,.F.);
#2873=ADVANCED_FACE('',(#443,#150,#151),#267,.F.);
#2874=ADVANCED_FACE('',(#444,#152,#153),#268,.T.);
#2875=ADVANCED_FACE('',(#445),#117,.F.);
#2876=ADVANCED_FACE('',(#446),#118,.F.);
#2877=ADVANCED_FACE('',(#447),#269,.T.);
#2878=ADVANCED_FACE('',(#448),#270,.T.);
#2879=ADVANCED_FACE('',(#449),#271,.T.);
#2880=ADVANCED_FACE('',(#450),#272,.T.);
#2881=ADVANCED_FACE('',(#451),#273,.T.);
#2882=ADVANCED_FACE('',(#452),#274,.T.);
#2883=ADVANCED_FACE('',(#453),#275,.T.);
#2884=ADVANCED_FACE('',(#454),#276,.T.);
#2885=ADVANCED_FACE('',(#455,#154,#155),#277,.T.);
#2886=ADVANCED_FACE('',(#456,#156,#157),#278,.F.);
#2887=ADVANCED_FACE('',(#457),#119,.F.);
#2888=ADVANCED_FACE('',(#458),#120,.F.);
#2889=ADVANCED_FACE('',(#459),#279,.F.);
#2890=ADVANCED_FACE('',(#460),#280,.F.);
#2891=ADVANCED_FACE('',(#461),#281,.F.);
#2892=ADVANCED_FACE('',(#462),#282,.F.);
#2893=ADVANCED_FACE('',(#463),#283,.F.);
#2894=ADVANCED_FACE('',(#464),#284,.F.);
#2895=ADVANCED_FACE('',(#465),#285,.F.);
#2896=ADVANCED_FACE('',(#466),#286,.F.);
#2897=ADVANCED_FACE('',(#467,#158,#159),#287,.F.);
#2898=ADVANCED_FACE('',(#468,#160,#161),#288,.T.);
#2899=ADVANCED_FACE('',(#469),#121,.F.);
#2900=ADVANCED_FACE('',(#470),#122,.F.);
#2901=ADVANCED_FACE('',(#471),#289,.T.);
#2902=ADVANCED_FACE('',(#472),#290,.T.);
#2903=ADVANCED_FACE('',(#473),#291,.T.);
#2904=ADVANCED_FACE('',(#474),#292,.T.);
#2905=ADVANCED_FACE('',(#475),#293,.T.);
#2906=ADVANCED_FACE('',(#476),#294,.T.);
#2907=ADVANCED_FACE('',(#477),#295,.T.);
#2908=ADVANCED_FACE('',(#478),#296,.T.);
#2909=ADVANCED_FACE('',(#479,#162,#163),#297,.T.);
#2910=ADVANCED_FACE('',(#480,#164,#165),#298,.F.);
#2911=CLOSED_SHELL('',(#2733,#2734,#2735,#2736,#2737,#2738,#2739,#2740,
#2741,#2742,#2743,#2744,#2745,#2746,#2747,#2748,#2749,#2750,#2751));
#2912=CLOSED_SHELL('',(#2752,#2753,#2754,#2755,#2756,#2757,#2758,#2759,
#2760,#2761,#2762,#2763,#2764,#2765,#2766,#2767,#2768,#2769,#2770));
#2913=CLOSED_SHELL('',(#2771,#2772,#2773,#2774,#2775,#2776,#2777,#2778,
#2779,#2780,#2781,#2782,#2783,#2784,#2785,#2786,#2787,#2788,#2789));
#2914=CLOSED_SHELL('',(#2790,#2791,#2792,#2793,#2794,#2795,#2796,#2797,
#2798,#2799,#2800,#2801,#2802,#2803,#2804,#2805,#2806,#2807,#2808));
#2915=CLOSED_SHELL('',(#2809,#2810,#2811,#2812,#2813,#2814,#2815,#2816,
#2817,#2818,#2819,#2820,#2821,#2822,#2823,#2824,#2825,#2826,#2827,#2828,
#2829,#2830,#2831,#2832,#2833,#2834,#2835,#2836,#2837,#2838,#2839,#2840));
#2916=CLOSED_SHELL('',(#2841,#2842,#2843,#2844,#2845,#2846,#2847,#2848,
#2849,#2850,#2851,#2852,#2853,#2854,#2855,#2856,#2857,#2858,#2859,#2860,
#2861,#2862));
#2917=CLOSED_SHELL('',(#2863,#2864,#2865,#2866,#2867,#2868,#2869,#2870,
#2871,#2872,#2873,#2874));
#2918=CLOSED_SHELL('',(#2875,#2876,#2877,#2878,#2879,#2880,#2881,#2882,
#2883,#2884,#2885,#2886));
#2919=CLOSED_SHELL('',(#2887,#2888,#2889,#2890,#2891,#2892,#2893,#2894,
#2895,#2896,#2897,#2898));
#2920=CLOSED_SHELL('',(#2899,#2900,#2901,#2902,#2903,#2904,#2905,#2906,
#2907,#2908,#2909,#2910));
#2921=DERIVED_UNIT_ELEMENT(#2941,1.);
#2922=DERIVED_UNIT_ELEMENT(#4996,-3.);
#2923=DERIVED_UNIT_ELEMENT(#2941,1.);
#2924=DERIVED_UNIT_ELEMENT(#4996,-3.);
#2925=DERIVED_UNIT_ELEMENT(#2941,1.);
#2926=DERIVED_UNIT_ELEMENT(#4996,-3.);
#2927=DERIVED_UNIT_ELEMENT(#2941,1.);
#2928=DERIVED_UNIT_ELEMENT(#4996,-3.);
#2929=DERIVED_UNIT_ELEMENT(#2941,1.);
#2930=DERIVED_UNIT_ELEMENT(#4996,-3.);
#2931=DERIVED_UNIT_ELEMENT(#2941,1.);
#2932=DERIVED_UNIT_ELEMENT(#4996,-3.);
#2933=DERIVED_UNIT_ELEMENT(#2941,1.);
#2934=DERIVED_UNIT_ELEMENT(#4996,-3.);
#2935=DERIVED_UNIT_ELEMENT(#2941,1.);
#2936=DERIVED_UNIT_ELEMENT(#4996,-3.);
#2937=DERIVED_UNIT_ELEMENT(#2941,1.);
#2938=DERIVED_UNIT_ELEMENT(#4996,-3.);
#2939=DERIVED_UNIT_ELEMENT(#2941,1.);
#2940=DERIVED_UNIT_ELEMENT(#4996,-3.);
#2941=(
MASS_UNIT()
NAMED_UNIT(*)
SI_UNIT(.KILO.,.GRAM.)
);
#2942=DERIVED_UNIT((#2921,#2922));
#2943=DERIVED_UNIT((#2923,#2924));
#2944=DERIVED_UNIT((#2925,#2926));
#2945=DERIVED_UNIT((#2927,#2928));
#2946=DERIVED_UNIT((#2929,#2930));
#2947=DERIVED_UNIT((#2931,#2932));
#2948=DERIVED_UNIT((#2933,#2934));
#2949=DERIVED_UNIT((#2935,#2936));
#2950=DERIVED_UNIT((#2937,#2938));
#2951=DERIVED_UNIT((#2939,#2940));
#2952=MEASURE_REPRESENTATION_ITEM('density measure',
POSITIVE_RATIO_MEASURE(7750.),#2942);
#2953=MEASURE_REPRESENTATION_ITEM('density measure',
POSITIVE_RATIO_MEASURE(7750.),#2943);
#2954=MEASURE_REPRESENTATION_ITEM('density measure',
POSITIVE_RATIO_MEASURE(7750.),#2944);
#2955=MEASURE_REPRESENTATION_ITEM('density measure',
POSITIVE_RATIO_MEASURE(7750.),#2945);
#2956=MEASURE_REPRESENTATION_ITEM('density measure',
POSITIVE_RATIO_MEASURE(7850.),#2946);
#2957=MEASURE_REPRESENTATION_ITEM('density measure',
POSITIVE_RATIO_MEASURE(7850.),#2947);
#2958=MEASURE_REPRESENTATION_ITEM('density measure',
POSITIVE_RATIO_MEASURE(7850.),#2948);
#2959=MEASURE_REPRESENTATION_ITEM('density measure',
POSITIVE_RATIO_MEASURE(7850.),#2949);
#2960=MEASURE_REPRESENTATION_ITEM('density measure',
POSITIVE_RATIO_MEASURE(7850.),#2950);
#2961=MEASURE_REPRESENTATION_ITEM('density measure',
POSITIVE_RATIO_MEASURE(7850.),#2951);
#2962=PROPERTY_DEFINITION_REPRESENTATION(#3012,#2982);
#2963=PROPERTY_DEFINITION_REPRESENTATION(#3013,#2983);
#2964=PROPERTY_DEFINITION_REPRESENTATION(#3014,#2984);
#2965=PROPERTY_DEFINITION_REPRESENTATION(#3015,#2985);
#2966=PROPERTY_DEFINITION_REPRESENTATION(#3016,#2986);
#2967=PROPERTY_DEFINITION_REPRESENTATION(#3017,#2987);
#2968=PROPERTY_DEFINITION_REPRESENTATION(#3018,#2988);
#2969=PROPERTY_DEFINITION_REPRESENTATION(#3019,#2989);
#2970=PROPERTY_DEFINITION_REPRESENTATION(#3020,#2990);
#2971=PROPERTY_DEFINITION_REPRESENTATION(#3021,#2991);
#2972=PROPERTY_DEFINITION_REPRESENTATION(#3022,#2992);
#2973=PROPERTY_DEFINITION_REPRESENTATION(#3023,#2993);
#2974=PROPERTY_DEFINITION_REPRESENTATION(#3024,#2994);
#2975=PROPERTY_DEFINITION_REPRESENTATION(#3025,#2995);
#2976=PROPERTY_DEFINITION_REPRESENTATION(#3026,#2996);
#2977=PROPERTY_DEFINITION_REPRESENTATION(#3027,#2997);
#2978=PROPERTY_DEFINITION_REPRESENTATION(#3028,#2998);
#2979=PROPERTY_DEFINITION_REPRESENTATION(#3029,#2999);
#2980=PROPERTY_DEFINITION_REPRESENTATION(#3030,#3000);
#2981=PROPERTY_DEFINITION_REPRESENTATION(#3031,#3001);
#2982=REPRESENTATION('material name',(#3002),#4984);
#2983=REPRESENTATION('density',(#2952),#4984);
#2984=REPRESENTATION('material name',(#3003),#4985);
#2985=REPRESENTATION('density',(#2953),#4985);
#2986=REPRESENTATION('material name',(#3004),#4986);
#2987=REPRESENTATION('density',(#2954),#4986);
#2988=REPRESENTATION('material name',(#3005),#4987);
#2989=REPRESENTATION('density',(#2955),#4987);
#2990=REPRESENTATION('material name',(#3006),#4988);
#2991=REPRESENTATION('density',(#2956),#4988);
#2992=REPRESENTATION('material name',(#3007),#4989);
#2993=REPRESENTATION('density',(#2957),#4989);
#2994=REPRESENTATION('material name',(#3008),#4990);
#2995=REPRESENTATION('density',(#2958),#4990);
#2996=REPRESENTATION('material name',(#3009),#4991);
#2997=REPRESENTATION('density',(#2959),#4991);
#2998=REPRESENTATION('material name',(#3010),#4992);
#2999=REPRESENTATION('density',(#2960),#4992);
#3000=REPRESENTATION('material name',(#3011),#4993);
#3001=REPRESENTATION('density',(#2961),#4993);
#3002=DESCRIPTIVE_REPRESENTATION_ITEM('Steel Grade 2, Plain',
'Steel Grade 2, Plain');
#3003=DESCRIPTIVE_REPRESENTATION_ITEM('Steel Grade 2, Plain',
'Steel Grade 2, Plain');
#3004=DESCRIPTIVE_REPRESENTATION_ITEM('Steel Grade 2, Plain',
'Steel Grade 2, Plain');
#3005=DESCRIPTIVE_REPRESENTATION_ITEM('Steel Grade 2, Plain',
'Steel Grade 2, Plain');
#3006=DESCRIPTIVE_REPRESENTATION_ITEM('Steel','Steel');
#3007=DESCRIPTIVE_REPRESENTATION_ITEM('Steel','Steel');
#3008=DESCRIPTIVE_REPRESENTATION_ITEM('Steel','Steel');
#3009=DESCRIPTIVE_REPRESENTATION_ITEM('Steel','Steel');
#3010=DESCRIPTIVE_REPRESENTATION_ITEM('Steel','Steel');
#3011=DESCRIPTIVE_REPRESENTATION_ITEM('Steel','Steel');
#3012=PROPERTY_DEFINITION('material property','material name',#5044);
#3013=PROPERTY_DEFINITION('material property','density of part',#5044);
#3014=PROPERTY_DEFINITION('material property','material name',#5045);
#3015=PROPERTY_DEFINITION('material property','density of part',#5045);
#3016=PROPERTY_DEFINITION('material property','material name',#5046);
#3017=PROPERTY_DEFINITION('material property','density of part',#5046);
#3018=PROPERTY_DEFINITION('material property','material name',#5047);
#3019=PROPERTY_DEFINITION('material property','density of part',#5047);
#3020=PROPERTY_DEFINITION('material property','material name',#5048);
#3021=PROPERTY_DEFINITION('material property','density of part',#5048);
#3022=PROPERTY_DEFINITION('material property','material name',#5049);
#3023=PROPERTY_DEFINITION('material property','density of part',#5049);
#3024=PROPERTY_DEFINITION('material property','material name',#5050);
#3025=PROPERTY_DEFINITION('material property','density of part',#5050);
#3026=PROPERTY_DEFINITION('material property','material name',#5051);
#3027=PROPERTY_DEFINITION('material property','density of part',#5051);
#3028=PROPERTY_DEFINITION('material property','material name',#5052);
#3029=PROPERTY_DEFINITION('material property','density of part',#5052);
#3030=PROPERTY_DEFINITION('material property','material name',#5053);
#3031=PROPERTY_DEFINITION('material property','density of part',#5053);
#3032=AXIS2_PLACEMENT_3D('',#4165,#3312,#3313);
#3033=AXIS2_PLACEMENT_3D('',#4166,#3314,#3315);
#3034=AXIS2_PLACEMENT_3D('',#4167,#3316,#3317);
#3035=AXIS2_PLACEMENT_3D('',#4169,#3318,#3319);
#3036=AXIS2_PLACEMENT_3D('',#4172,#3321,#3322);
#3037=AXIS2_PLACEMENT_3D('',#4173,#3323,#3324);
#3038=AXIS2_PLACEMENT_3D('',#4175,#3325,#3326);
#3039=AXIS2_PLACEMENT_3D('',#4177,#3327,#3328);
#3040=AXIS2_PLACEMENT_3D('',#4178,#3329,#3330);
#3041=AXIS2_PLACEMENT_3D('',#4179,#3331,#3332);
#3042=AXIS2_PLACEMENT_3D('',#4192,#3339,#3340);
#3043=AXIS2_PLACEMENT_3D('',#4194,#3341,#3342);
#3044=AXIS2_PLACEMENT_3D('',#4196,#3344,#3345);
#3045=AXIS2_PLACEMENT_3D('',#4203,#3349,#3350);
#3046=AXIS2_PLACEMENT_3D('',#4207,#3353,#3354);
#3047=AXIS2_PLACEMENT_3D('',#4211,#3357,#3358);
#3048=AXIS2_PLACEMENT_3D('',#4215,#3361,#3362);
#3049=AXIS2_PLACEMENT_3D('',#4219,#3365,#3366);
#3050=AXIS2_PLACEMENT_3D('',#4221,#3368,#3369);
#3051=AXIS2_PLACEMENT_3D('',#4224,#3372,#3373);
#3052=AXIS2_PLACEMENT_3D('',#4226,#3375,#3376);
#3053=AXIS2_PLACEMENT_3D('',#4228,#3378,#3379);
#3054=AXIS2_PLACEMENT_3D('',#4230,#3381,#3382);
#3055=AXIS2_PLACEMENT_3D('',#4232,#3384,#3385);
#3056=AXIS2_PLACEMENT_3D('',#4233,#3386,#3387);
#3057=AXIS2_PLACEMENT_3D('',#4236,#3389,#3390);
#3058=AXIS2_PLACEMENT_3D('',#4237,#3391,#3392);
#3059=AXIS2_PLACEMENT_3D('',#4238,#3393,#3394);
#3060=AXIS2_PLACEMENT_3D('',#4239,#3395,#3396);
#3061=AXIS2_PLACEMENT_3D('',#4240,#3397,#3398);
#3062=AXIS2_PLACEMENT_3D('',#4242,#3399,#3400);
#3063=AXIS2_PLACEMENT_3D('',#4245,#3402,#3403);
#3064=AXIS2_PLACEMENT_3D('',#4246,#3404,#3405);
#3065=AXIS2_PLACEMENT_3D('',#4248,#3406,#3407);
#3066=AXIS2_PLACEMENT_3D('',#4250,#3408,#3409);
#3067=AXIS2_PLACEMENT_3D('',#4251,#3410,#3411);
#3068=AXIS2_PLACEMENT_3D('',#4252,#3412,#3413);
#3069=AXIS2_PLACEMENT_3D('',#4265,#3420,#3421);
#3070=AXIS2_PLACEMENT_3D('',#4267,#3422,#3423);
#3071=AXIS2_PLACEMENT_3D('',#4269,#3425,#3426);
#3072=AXIS2_PLACEMENT_3D('',#4276,#3430,#3431);
#3073=AXIS2_PLACEMENT_3D('',#4280,#3434,#3435);
#3074=AXIS2_PLACEMENT_3D('',#4284,#3438,#3439);
#3075=AXIS2_PLACEMENT_3D('',#4288,#3442,#3443);
#3076=AXIS2_PLACEMENT_3D('',#4292,#3446,#3447);
#3077=AXIS2_PLACEMENT_3D('',#4294,#3449,#3450);
#3078=AXIS2_PLACEMENT_3D('',#4297,#3453,#3454);
#3079=AXIS2_PLACEMENT_3D('',#4299,#3456,#3457);
#3080=AXIS2_PLACEMENT_3D('',#4301,#3459,#3460);
#3081=AXIS2_PLACEMENT_3D('',#4303,#3462,#3463);
#3082=AXIS2_PLACEMENT_3D('',#4305,#3465,#3466);
#3083=AXIS2_PLACEMENT_3D('',#4306,#3467,#3468);
#3084=AXIS2_PLACEMENT_3D('',#4309,#3470,#3471);
#3085=AXIS2_PLACEMENT_3D('',#4310,#3472,#3473);
#3086=AXIS2_PLACEMENT_3D('',#4311,#3474,#3475);
#3087=AXIS2_PLACEMENT_3D('',#4312,#3476,#3477);
#3088=AXIS2_PLACEMENT_3D('',#4313,#3478,#3479);
#3089=AXIS2_PLACEMENT_3D('',#4315,#3480,#3481);
#3090=AXIS2_PLACEMENT_3D('',#4318,#3483,#3484);
#3091=AXIS2_PLACEMENT_3D('',#4319,#3485,#3486);
#3092=AXIS2_PLACEMENT_3D('',#4321,#3487,#3488);
#3093=AXIS2_PLACEMENT_3D('',#4323,#3489,#3490);
#3094=AXIS2_PLACEMENT_3D('',#4324,#3491,#3492);
#3095=AXIS2_PLACEMENT_3D('',#4325,#3493,#3494);
#3096=AXIS2_PLACEMENT_3D('',#4338,#3501,#3502);
#3097=AXIS2_PLACEMENT_3D('',#4340,#3503,#3504);
#3098=AXIS2_PLACEMENT_3D('',#4342,#3506,#3507);
#3099=AXIS2_PLACEMENT_3D('',#4349,#3511,#3512);
#3100=AXIS2_PLACEMENT_3D('',#4353,#3515,#3516);
#3101=AXIS2_PLACEMENT_3D('',#4357,#3519,#3520);
#3102=AXIS2_PLACEMENT_3D('',#4361,#3523,#3524);
#3103=AXIS2_PLACEMENT_3D('',#4365,#3527,#3528);
#3104=AXIS2_PLACEMENT_3D('',#4367,#3530,#3531);
#3105=AXIS2_PLACEMENT_3D('',#4370,#3534,#3535);
#3106=AXIS2_PLACEMENT_3D('',#4372,#3537,#3538);
#3107=AXIS2_PLACEMENT_3D('',#4374,#3540,#3541);
#3108=AXIS2_PLACEMENT_3D('',#4376,#3543,#3544);
#3109=AXIS2_PLACEMENT_3D('',#4378,#3546,#3547);
#3110=AXIS2_PLACEMENT_3D('',#4379,#3548,#3549);
#3111=AXIS2_PLACEMENT_3D('',#4382,#3551,#3552);
#3112=AXIS2_PLACEMENT_3D('',#4383,#3553,#3554);
#3113=AXIS2_PLACEMENT_3D('',#4384,#3555,#3556);
#3114=AXIS2_PLACEMENT_3D('',#4385,#3557,#3558);
#3115=AXIS2_PLACEMENT_3D('',#4386,#3559,#3560);
#3116=AXIS2_PLACEMENT_3D('',#4388,#3561,#3562);
#3117=AXIS2_PLACEMENT_3D('',#4391,#3564,#3565);
#3118=AXIS2_PLACEMENT_3D('',#4392,#3566,#3567);
#3119=AXIS2_PLACEMENT_3D('',#4394,#3568,#3569);
#3120=AXIS2_PLACEMENT_3D('',#4396,#3570,#3571);
#3121=AXIS2_PLACEMENT_3D('',#4397,#3572,#3573);
#3122=AXIS2_PLACEMENT_3D('',#4398,#3574,#3575);
#3123=AXIS2_PLACEMENT_3D('',#4411,#3582,#3583);
#3124=AXIS2_PLACEMENT_3D('',#4413,#3584,#3585);
#3125=AXIS2_PLACEMENT_3D('',#4415,#3587,#3588);
#3126=AXIS2_PLACEMENT_3D('',#4422,#3592,#3593);
#3127=AXIS2_PLACEMENT_3D('',#4426,#3596,#3597);
#3128=AXIS2_PLACEMENT_3D('',#4430,#3600,#3601);
#3129=AXIS2_PLACEMENT_3D('',#4434,#3604,#3605);
#3130=AXIS2_PLACEMENT_3D('',#4438,#3608,#3609);
#3131=AXIS2_PLACEMENT_3D('',#4440,#3611,#3612);
#3132=AXIS2_PLACEMENT_3D('',#4443,#3615,#3616);
#3133=AXIS2_PLACEMENT_3D('',#4445,#3618,#3619);
#3134=AXIS2_PLACEMENT_3D('',#4447,#3621,#3622);
#3135=AXIS2_PLACEMENT_3D('',#4449,#3624,#3625);
#3136=AXIS2_PLACEMENT_3D('',#4451,#3627,#3628);
#3137=AXIS2_PLACEMENT_3D('',#4452,#3629,#3630);
#3138=AXIS2_PLACEMENT_3D('',#4455,#3632,#3633);
#3139=AXIS2_PLACEMENT_3D('',#4456,#3634,#3635);
#3140=AXIS2_PLACEMENT_3D('',#4457,#3636,#3637);
#3141=AXIS2_PLACEMENT_3D('',#4458,#3638,#3639);
#3142=AXIS2_PLACEMENT_3D('',#4459,#3640,#3641);
#3143=AXIS2_PLACEMENT_3D('',#4461,#3642,#3643);
#3144=AXIS2_PLACEMENT_3D('',#4464,#3645,#3646);
#3145=AXIS2_PLACEMENT_3D('',#4465,#3647,#3648);
#3146=AXIS2_PLACEMENT_3D('',#4475,#3653,#3654);
#3147=AXIS2_PLACEMENT_3D('',#4477,#3655,#3656);
#3148=AXIS2_PLACEMENT_3D('',#4479,#3657,#3658);
#3149=AXIS2_PLACEMENT_3D('',#4481,#3659,#3660);
#3150=AXIS2_PLACEMENT_3D('',#4482,#3661,#3662);
#3151=AXIS2_PLACEMENT_3D('',#4484,#3663,#3664);
#3152=AXIS2_PLACEMENT_3D('',#4486,#3666,#3667);
#3153=AXIS2_PLACEMENT_3D('',#4488,#3668,#3669);
#3154=AXIS2_PLACEMENT_3D('',#4490,#3671,#3672);
#3155=AXIS2_PLACEMENT_3D('',#4492,#3673,#3674);
#3156=AXIS2_PLACEMENT_3D('',#4494,#3676,#3677);
#3157=AXIS2_PLACEMENT_3D('',#4496,#3678,#3679);
#3158=AXIS2_PLACEMENT_3D('',#4498,#3681,#3682);
#3159=AXIS2_PLACEMENT_3D('',#4500,#3683,#3684);
#3160=AXIS2_PLACEMENT_3D('',#4502,#3686,#3687);
#3161=AXIS2_PLACEMENT_3D('',#4504,#3688,#3689);
#3162=AXIS2_PLACEMENT_3D('',#4506,#3691,#3692);
#3163=AXIS2_PLACEMENT_3D('',#4508,#3693,#3694);
#3164=AXIS2_PLACEMENT_3D('',#4510,#3696,#3697);
#3165=AXIS2_PLACEMENT_3D('',#4512,#3698,#3699);
#3166=AXIS2_PLACEMENT_3D('',#4514,#3701,#3702);
#3167=AXIS2_PLACEMENT_3D('',#4516,#3703,#3704);
#3168=AXIS2_PLACEMENT_3D('',#4518,#3706,#3707);
#3169=AXIS2_PLACEMENT_3D('',#4520,#3708,#3709);
#3170=AXIS2_PLACEMENT_3D('',#4523,#3711,#3712);
#3171=AXIS2_PLACEMENT_3D('',#4524,#3713,#3714);
#3172=AXIS2_PLACEMENT_3D('',#4525,#3715,#3716);
#3173=AXIS2_PLACEMENT_3D('',#4527,#3717,#3718);
#3174=AXIS2_PLACEMENT_3D('',#4530,#3720,#3721);
#3175=AXIS2_PLACEMENT_3D('',#4531,#3722,#3723);
#3176=AXIS2_PLACEMENT_3D('',#4532,#3724,#3725);
#3177=AXIS2_PLACEMENT_3D('',#4534,#3726,#3727);
#3178=AXIS2_PLACEMENT_3D('',#4537,#3729,#3730);
#3179=AXIS2_PLACEMENT_3D('',#4538,#3731,#3732);
#3180=AXIS2_PLACEMENT_3D('',#4539,#3733,#3734);
#3181=AXIS2_PLACEMENT_3D('',#4541,#3735,#3736);
#3182=AXIS2_PLACEMENT_3D('',#4544,#3738,#3739);
#3183=AXIS2_PLACEMENT_3D('',#4545,#3740,#3741);
#3184=AXIS2_PLACEMENT_3D('',#4546,#3742,#3743);
#3185=AXIS2_PLACEMENT_3D('',#4548,#3744,#3745);
#3186=AXIS2_PLACEMENT_3D('',#4551,#3747,#3748);
#3187=AXIS2_PLACEMENT_3D('',#4552,#3749,#3750);
#3188=AXIS2_PLACEMENT_3D('',#4553,#3751,#3752);
#3189=AXIS2_PLACEMENT_3D('',#4562,#3757,#3758);
#3190=AXIS2_PLACEMENT_3D('',#4564,#3759,#3760);
#3191=AXIS2_PLACEMENT_3D('',#4567,#3762,#3763);
#3192=AXIS2_PLACEMENT_3D('',#4568,#3764,#3765);
#3193=AXIS2_PLACEMENT_3D('',#4571,#3768,#3769);
#3194=AXIS2_PLACEMENT_3D('',#4577,#3773,#3774);
#3195=AXIS2_PLACEMENT_3D('',#4584,#3777,#3778);
#3196=AXIS2_PLACEMENT_3D('',#4587,#3781,#3782);
#3197=AXIS2_PLACEMENT_3D('',#4593,#3786,#3787);
#3198=AXIS2_PLACEMENT_3D('',#4595,#3788,#3789);
#3199=AXIS2_PLACEMENT_3D('',#4597,#3791,#3792);
#3200=AXIS2_PLACEMENT_3D('',#4599,#3794,#3795);
#3201=AXIS2_PLACEMENT_3D('',#4603,#3798,#3799);
#3202=AXIS2_PLACEMENT_3D('',#4605,#3801,#3802);
#3203=AXIS2_PLACEMENT_3D('',#4606,#3803,#3804);
#3204=AXIS2_PLACEMENT_3D('',#4607,#3805,#3806);
#3205=AXIS2_PLACEMENT_3D('',#4609,#3807,#3808);
#3206=AXIS2_PLACEMENT_3D('',#4612,#3810,#3811);
#3207=AXIS2_PLACEMENT_3D('',#4613,#3812,#3813);
#3208=AXIS2_PLACEMENT_3D('',#4614,#3814,#3815);
#3209=AXIS2_PLACEMENT_3D('',#4616,#3816,#3817);
#3210=AXIS2_PLACEMENT_3D('',#4619,#3819,#3820);
#3211=AXIS2_PLACEMENT_3D('',#4620,#3821,#3822);
#3212=AXIS2_PLACEMENT_3D('',#4621,#3823,#3824);
#3213=AXIS2_PLACEMENT_3D('',#4623,#3825,#3826);
#3214=AXIS2_PLACEMENT_3D('',#4626,#3828,#3829);
#3215=AXIS2_PLACEMENT_3D('',#4627,#3830,#3831);
#3216=AXIS2_PLACEMENT_3D('',#4628,#3832,#3833);
#3217=AXIS2_PLACEMENT_3D('',#4630,#3834,#3835);
#3218=AXIS2_PLACEMENT_3D('',#4633,#3837,#3838);
#3219=AXIS2_PLACEMENT_3D('',#4634,#3839,#3840);
#3220=AXIS2_PLACEMENT_3D('',#4635,#3841,#3842);
#3221=AXIS2_PLACEMENT_3D('',#4660,#3855,#3856);
#3222=AXIS2_PLACEMENT_3D('',#4666,#3860,#3861);
#3223=AXIS2_PLACEMENT_3D('',#4670,#3864,#3865);
#3224=AXIS2_PLACEMENT_3D('',#4674,#3868,#3869);
#3225=AXIS2_PLACEMENT_3D('',#4678,#3872,#3873);
#3226=AXIS2_PLACEMENT_3D('',#4682,#3876,#3877);
#3227=AXIS2_PLACEMENT_3D('',#4686,#3880,#3881);
#3228=AXIS2_PLACEMENT_3D('',#4690,#3884,#3885);
#3229=AXIS2_PLACEMENT_3D('',#4694,#3888,#3889);
#3230=AXIS2_PLACEMENT_3D('',#4698,#3892,#3893);
#3231=AXIS2_PLACEMENT_3D('',#4702,#3896,#3897);
#3232=AXIS2_PLACEMENT_3D('',#4706,#3900,#3901);
#3233=AXIS2_PLACEMENT_3D('',#4708,#3903,#3904);
#3234=AXIS2_PLACEMENT_3D('',#4709,#3905,#3906);
#3235=AXIS2_PLACEMENT_3D('',#4710,#3907,#3908);
#3236=AXIS2_PLACEMENT_3D('',#4712,#3909,#3910);
#3237=AXIS2_PLACEMENT_3D('',#4715,#3912,#3913);
#3238=AXIS2_PLACEMENT_3D('',#4716,#3914,#3915);
#3239=AXIS2_PLACEMENT_3D('',#4718,#3916,#3917);
#3240=AXIS2_PLACEMENT_3D('',#4721,#3919,#3920);
#3241=AXIS2_PLACEMENT_3D('',#4722,#3921,#3922);
#3242=AXIS2_PLACEMENT_3D('',#4731,#3927,#3928);
#3243=AXIS2_PLACEMENT_3D('',#4737,#3932,#3933);
#3244=AXIS2_PLACEMENT_3D('',#4743,#3937,#3938);
#3245=AXIS2_PLACEMENT_3D('',#4749,#3942,#3943);
#3246=AXIS2_PLACEMENT_3D('',#4755,#3947,#3948);
#3247=AXIS2_PLACEMENT_3D('',#4761,#3952,#3953);
#3248=AXIS2_PLACEMENT_3D('',#4767,#3957,#3958);
#3249=AXIS2_PLACEMENT_3D('',#4770,#3961,#3962);
#3250=AXIS2_PLACEMENT_3D('',#4771,#3963,#3964);
#3251=AXIS2_PLACEMENT_3D('',#4772,#3965,#3966);
#3252=AXIS2_PLACEMENT_3D('',#4773,#3967,#3968);
#3253=AXIS2_PLACEMENT_3D('',#4775,#3969,#3970);
#3254=AXIS2_PLACEMENT_3D('',#4778,#3972,#3973);
#3255=AXIS2_PLACEMENT_3D('',#4779,#3974,#3975);
#3256=AXIS2_PLACEMENT_3D('',#4781,#3976,#3977);
#3257=AXIS2_PLACEMENT_3D('',#4784,#3979,#3980);
#3258=AXIS2_PLACEMENT_3D('',#4785,#3981,#3982);
#3259=AXIS2_PLACEMENT_3D('',#4794,#3987,#3988);
#3260=AXIS2_PLACEMENT_3D('',#4800,#3992,#3993);
#3261=AXIS2_PLACEMENT_3D('',#4806,#3997,#3998);
#3262=AXIS2_PLACEMENT_3D('',#4812,#4002,#4003);
#3263=AXIS2_PLACEMENT_3D('',#4818,#4007,#4008);
#3264=AXIS2_PLACEMENT_3D('',#4824,#4012,#4013);
#3265=AXIS2_PLACEMENT_3D('',#4830,#4017,#4018);
#3266=AXIS2_PLACEMENT_3D('',#4833,#4021,#4022);
#3267=AXIS2_PLACEMENT_3D('',#4834,#4023,#4024);
#3268=AXIS2_PLACEMENT_3D('',#4835,#4025,#4026);
#3269=AXIS2_PLACEMENT_3D('',#4836,#4027,#4028);
#3270=AXIS2_PLACEMENT_3D('',#4838,#4029,#4030);
#3271=AXIS2_PLACEMENT_3D('',#4841,#4032,#4033);
#3272=AXIS2_PLACEMENT_3D('',#4842,#4034,#4035);
#3273=AXIS2_PLACEMENT_3D('',#4844,#4036,#4037);
#3274=AXIS2_PLACEMENT_3D('',#4847,#4039,#4040);
#3275=AXIS2_PLACEMENT_3D('',#4848,#4041,#4042);
#3276=AXIS2_PLACEMENT_3D('',#4857,#4047,#4048);
#3277=AXIS2_PLACEMENT_3D('',#4863,#4052,#4053);
#3278=AXIS2_PLACEMENT_3D('',#4869,#4057,#4058);
#3279=AXIS2_PLACEMENT_3D('',#4875,#4062,#4063);
#3280=AXIS2_PLACEMENT_3D('',#4881,#4067,#4068);
#3281=AXIS2_PLACEMENT_3D('',#4887,#4072,#4073);
#3282=AXIS2_PLACEMENT_3D('',#4893,#4077,#4078);
#3283=AXIS2_PLACEMENT_3D('',#4896,#4081,#4082);
#3284=AXIS2_PLACEMENT_3D('',#4897,#4083,#4084);
#3285=AXIS2_PLACEMENT_3D('',#4898,#4085,#4086);
#3286=AXIS2_PLACEMENT_3D('',#4899,#4087,#4088);
#3287=AXIS2_PLACEMENT_3D('',#4901,#4089,#4090);
#3288=AXIS2_PLACEMENT_3D('',#4904,#4092,#4093);
#3289=AXIS2_PLACEMENT_3D('',#4905,#4094,#4095);
#3290=AXIS2_PLACEMENT_3D('',#4907,#4096,#4097);
#3291=AXIS2_PLACEMENT_3D('',#4910,#4099,#4100);
#3292=AXIS2_PLACEMENT_3D('',#4911,#4101,#4102);
#3293=AXIS2_PLACEMENT_3D('',#4920,#4107,#4108);
#3294=AXIS2_PLACEMENT_3D('',#4926,#4112,#4113);
#3295=AXIS2_PLACEMENT_3D('',#4932,#4117,#4118);
#3296=AXIS2_PLACEMENT_3D('',#4938,#4122,#4123);
#3297=AXIS2_PLACEMENT_3D('',#4944,#4127,#4128);
#3298=AXIS2_PLACEMENT_3D('',#4950,#4132,#4133);
#3299=AXIS2_PLACEMENT_3D('',#4956,#4137,#4138);
#3300=AXIS2_PLACEMENT_3D('',#4959,#4141,#4142);
#3301=AXIS2_PLACEMENT_3D('',#4960,#4143,#4144);
#3302=AXIS2_PLACEMENT_3D('',#4961,#4145,#4146);
#3303=AXIS2_PLACEMENT_3D('',#4962,#4147,#4148);
#3304=AXIS2_PLACEMENT_3D('',#4963,#4149,#4150);
#3305=AXIS2_PLACEMENT_3D('',#4964,#4151,#4152);
#3306=AXIS2_PLACEMENT_3D('',#4965,#4153,#4154);
#3307=AXIS2_PLACEMENT_3D('',#4966,#4155,#4156);
#3308=AXIS2_PLACEMENT_3D('',#4967,#4157,#4158);
#3309=AXIS2_PLACEMENT_3D('',#4968,#4159,#4160);
#3310=AXIS2_PLACEMENT_3D('',#4969,#4161,#4162);
#3311=AXIS2_PLACEMENT_3D('',#4970,#4163,#4164);
#3312=DIRECTION('axis',(0.,0.,1.));
#3313=DIRECTION('refdir',(1.,0.,0.));
#3314=DIRECTION('axis',(0.,0.,1.));
#3315=DIRECTION('refdir',(1.,0.,0.));
#3316=DIRECTION('center_axis',(0.,0.,1.));
#3317=DIRECTION('ref_axis',(-1.,0.,0.));
#3318=DIRECTION('center_axis',(-1.06387651071382E-15,0.,1.));
#3319=DIRECTION('ref_axis',(-1.,0.,-1.06387651071382E-15));
#3320=DIRECTION('',(-0.73423251512767,-8.99175499481012E-17,-0.678898087881602));
#3321=DIRECTION('center_axis',(1.06387651071382E-15,0.,-1.));
#3322=DIRECTION('ref_axis',(-1.,0.,-1.06387651071382E-15));
#3323=DIRECTION('center_axis',(1.06387651071382E-15,0.,-1.));
#3324=DIRECTION('ref_axis',(-1.,0.,-1.05179023385541E-15));
#3325=DIRECTION('center_axis',(-1.06387651071382E-15,0.,1.));
#3326=DIRECTION('ref_axis',(1.,0.,1.06387651071382E-15));
#3327=DIRECTION('center_axis',(-1.22464679914735E-16,-1.,-1.30287296353373E-31));
#3328=DIRECTION('ref_axis',(1.,-1.22464679914735E-16,1.02257383847054E-15));
#3329=DIRECTION('center_axis',(1.06387651071382E-15,0.,-1.));
#3330=DIRECTION('ref_axis',(1.,0.,1.06387651071382E-15));
#3331=DIRECTION('center_axis',(-1.06387651071382E-15,0.,1.));
#3332=DIRECTION('ref_axis',(1.,0.,1.06387651071382E-15));
#3333=DIRECTION('',(-0.866025403784439,-0.5,-9.21344084767719E-16));
#3334=DIRECTION('',(-0.866025403784439,0.5,-9.21344084767719E-16));
#3335=DIRECTION('',(6.40987562127854E-16,1.,6.81931611007542E-31));
#3336=DIRECTION('',(0.866025403784439,0.5,9.21344084767719E-16));
#3337=DIRECTION('',(0.866025403784439,-0.5,9.21344084767719E-16));
#3338=DIRECTION('',(-1.60246890531964E-16,-1.,-1.70482902751885E-31));
#3339=DIRECTION('center_axis',(1.06387651071382E-15,0.,-1.));
#3340=DIRECTION('ref_axis',(-1.,0.,-1.06387651071382E-15));
#3341=DIRECTION('center_axis',(1.06387651071382E-15,0.,-1.));
#3342=DIRECTION('ref_axis',(1.,0.,1.06387651071382E-15));
#3343=DIRECTION('',(-1.06387651071382E-15,0.,1.));
#3344=DIRECTION('center_axis',(0.0435778713738291,-0.0754790873051733,-0.996194698091746));
#3345=DIRECTION('ref_axis',(-0.866025403784439,-0.5,-3.35810244624808E-17));
#3346=DIRECTION('',(0.,0.997141949694316,-0.0755508581011305));
#3347=DIRECTION('',(-0.866025403784439,-0.5,0.));
#3348=DIRECTION('',(-0.863550259614423,0.498570974847158,-0.0755508581011305));
#3349=DIRECTION('center_axis',(0.0871557427476581,-1.3966436767316E-17,
-0.996194698091746));
#3350=DIRECTION('ref_axis',(-1.60246890531964E-16,-1.,1.77292017095641E-32));
#3351=DIRECTION('',(-1.60246890531964E-16,-1.,0.));
#3352=DIRECTION('',(-0.863550259614423,-0.498570974847158,-0.0755508581011305));
#3353=DIRECTION('center_axis',(0.0435778713738291,0.0754790873051733,-0.996194698091746));
#3354=DIRECTION('ref_axis',(0.866025403784439,-0.5,3.35810244624808E-17));
#3355=DIRECTION('',(0.866025403784439,-0.5,0.));
#3356=DIRECTION('',(-1.59381164582915E-16,-0.997141949694316,-0.0755508581011305));
#3357=DIRECTION('center_axis',(-0.0435778713738291,0.0754790873051733,-0.996194698091746));
#3358=DIRECTION('ref_axis',(0.866025403784439,0.5,-3.35810244624808E-17));
#3359=DIRECTION('',(0.866025403784439,0.5,0.));
#3360=DIRECTION('',(0.863550259614423,-0.498570974847159,-0.0755508581011305));
#3361=DIRECTION('center_axis',(-0.0871557427476581,5.58657470692638E-17,
-0.996194698091746));
#3362=DIRECTION('ref_axis',(6.40987562127854E-16,1.,4.7015367027096E-32));
#3363=DIRECTION('',(6.40987562127854E-16,1.,0.));
#3364=DIRECTION('',(0.863550259614423,0.498570974847158,-0.0755508581011305));
#3365=DIRECTION('center_axis',(-0.0435778713738291,-0.0754790873051733,
-0.996194698091746));
#3366=DIRECTION('ref_axis',(-0.866025403784439,0.5,3.35810244624808E-17));
#3367=DIRECTION('',(-0.866025403784439,0.5,0.));
#3368=DIRECTION('center_axis',(0.5,-0.866025403784439,0.));
#3369=DIRECTION('ref_axis',(-0.866025403784439,-0.5,0.));
#3370=DIRECTION('',(0.,0.,-1.));
#3371=DIRECTION('',(0.,0.,-1.));
#3372=DIRECTION('center_axis',(1.,-1.60246890531964E-16,0.));
#3373=DIRECTION('ref_axis',(-1.60246890531964E-16,-1.,0.));
#3374=DIRECTION('',(0.,0.,-1.));
#3375=DIRECTION('center_axis',(0.5,0.866025403784439,0.));
#3376=DIRECTION('ref_axis',(0.866025403784439,-0.5,0.));
#3377=DIRECTION('',(0.,0.,-1.));
#3378=DIRECTION('center_axis',(-0.5,0.866025403784439,0.));
#3379=DIRECTION('ref_axis',(0.866025403784439,0.5,0.));
#3380=DIRECTION('',(0.,0.,-1.));
#3381=DIRECTION('center_axis',(-1.,6.40987562127854E-16,0.));
#3382=DIRECTION('ref_axis',(6.40987562127854E-16,1.,0.));
#3383=DIRECTION('',(0.,0.,-1.));
#3384=DIRECTION('center_axis',(-0.5,-0.866025403784439,0.));
#3385=DIRECTION('ref_axis',(-0.866025403784439,0.5,0.));
#3386=DIRECTION('center_axis',(1.06387651071382E-15,0.,-1.));
#3387=DIRECTION('ref_axis',(-1.,0.,-1.06387651071382E-15));
#3388=DIRECTION('',(-1.06387651071382E-15,0.,1.));
#3389=DIRECTION('center_axis',(-1.06387651071382E-15,0.,1.));
#3390=DIRECTION('ref_axis',(-1.,0.,-1.06387651071382E-15));
#3391=DIRECTION('center_axis',(1.06387651071382E-15,0.,-1.));
#3392=DIRECTION('ref_axis',(-1.,0.,-1.06387651071382E-15));
#3393=DIRECTION('center_axis',(1.06387651071382E-15,0.,-1.));
#3394=DIRECTION('ref_axis',(-1.,0.,-1.06387651071382E-15));
#3395=DIRECTION('axis',(0.,0.,1.));
#3396=DIRECTION('refdir',(1.,0.,0.));
#3397=DIRECTION('center_axis',(0.,0.,1.));
#3398=DIRECTION('ref_axis',(-1.,0.,0.));
#3399=DIRECTION('center_axis',(-1.06387651071382E-15,0.,1.));
#3400=DIRECTION('ref_axis',(-1.,0.,-1.06387651071382E-15));
#3401=DIRECTION('',(-0.73423251512767,-8.99175499481012E-17,-0.678898087881602));
#3402=DIRECTION('center_axis',(1.06387651071382E-15,0.,-1.));
#3403=DIRECTION('ref_axis',(-1.,0.,-1.06387651071382E-15));
#3404=DIRECTION('center_axis',(1.06387651071382E-15,0.,-1.));
#3405=DIRECTION('ref_axis',(-1.,0.,-1.05179023385541E-15));
#3406=DIRECTION('center_axis',(-1.06387651071382E-15,0.,1.));
#3407=DIRECTION('ref_axis',(1.,0.,1.06387651071382E-15));
#3408=DIRECTION('center_axis',(-1.22464679914735E-16,-1.,-1.30287296353373E-31));
#3409=DIRECTION('ref_axis',(1.,-1.22464679914735E-16,1.02257383847054E-15));
#3410=DIRECTION('center_axis',(1.06387651071382E-15,0.,-1.));
#3411=DIRECTION('ref_axis',(1.,0.,1.06387651071382E-15));
#3412=DIRECTION('center_axis',(-1.06387651071382E-15,0.,1.));
#3413=DIRECTION('ref_axis',(1.,0.,1.06387651071382E-15));
#3414=DIRECTION('',(-0.866025403784439,-0.5,-9.21344084767719E-16));
#3415=DIRECTION('',(-0.866025403784439,0.5,-9.21344084767719E-16));
#3416=DIRECTION('',(6.40987562127854E-16,1.,6.81931611007542E-31));
#3417=DIRECTION('',(0.866025403784439,0.5,9.21344084767719E-16));
#3418=DIRECTION('',(0.866025403784439,-0.5,9.21344084767719E-16));
#3419=DIRECTION('',(-1.60246890531964E-16,-1.,-1.70482902751885E-31));
#3420=DIRECTION('center_axis',(1.06387651071382E-15,0.,-1.));
#3421=DIRECTION('ref_axis',(-1.,0.,-1.06387651071382E-15));
#3422=DIRECTION('center_axis',(1.06387651071382E-15,0.,-1.));
#3423=DIRECTION('ref_axis',(1.,0.,1.06387651071382E-15));
#3424=DIRECTION('',(-1.06387651071382E-15,0.,1.));
#3425=DIRECTION('center_axis',(0.0435778713738291,-0.0754790873051733,-0.996194698091746));
#3426=DIRECTION('ref_axis',(-0.866025403784439,-0.5,-3.35810244624808E-17));
#3427=DIRECTION('',(0.,0.997141949694316,-0.0755508581011305));
#3428=DIRECTION('',(-0.866025403784439,-0.5,0.));
#3429=DIRECTION('',(-0.863550259614423,0.498570974847158,-0.0755508581011305));
#3430=DIRECTION('center_axis',(0.0871557427476581,-1.3966436767316E-17,
-0.996194698091746));
#3431=DIRECTION('ref_axis',(-1.60246890531964E-16,-1.,1.77292017095641E-32));
#3432=DIRECTION('',(-1.60246890531964E-16,-1.,0.));
#3433=DIRECTION('',(-0.863550259614423,-0.498570974847158,-0.0755508581011305));
#3434=DIRECTION('center_axis',(0.0435778713738291,0.0754790873051733,-0.996194698091746));
#3435=DIRECTION('ref_axis',(0.866025403784439,-0.5,3.35810244624808E-17));
#3436=DIRECTION('',(0.866025403784439,-0.5,0.));
#3437=DIRECTION('',(-1.59381164582915E-16,-0.997141949694316,-0.0755508581011305));
#3438=DIRECTION('center_axis',(-0.0435778713738291,0.0754790873051733,-0.996194698091746));
#3439=DIRECTION('ref_axis',(0.866025403784439,0.5,-3.35810244624808E-17));
#3440=DIRECTION('',(0.866025403784439,0.5,0.));
#3441=DIRECTION('',(0.863550259614423,-0.498570974847159,-0.0755508581011305));
#3442=DIRECTION('center_axis',(-0.0871557427476581,5.58657470692638E-17,
-0.996194698091746));
#3443=DIRECTION('ref_axis',(6.40987562127854E-16,1.,4.7015367027096E-32));
#3444=DIRECTION('',(6.40987562127854E-16,1.,0.));
#3445=DIRECTION('',(0.863550259614423,0.498570974847158,-0.0755508581011305));
#3446=DIRECTION('center_axis',(-0.0435778713738291,-0.0754790873051733,
-0.996194698091746));
#3447=DIRECTION('ref_axis',(-0.866025403784439,0.5,3.35810244624808E-17));
#3448=DIRECTION('',(-0.866025403784439,0.5,0.));
#3449=DIRECTION('center_axis',(0.5,-0.866025403784439,0.));
#3450=DIRECTION('ref_axis',(-0.866025403784439,-0.5,0.));
#3451=DIRECTION('',(0.,0.,-1.));
#3452=DIRECTION('',(0.,0.,-1.));
#3453=DIRECTION('center_axis',(1.,-1.60246890531964E-16,0.));
#3454=DIRECTION('ref_axis',(-1.60246890531964E-16,-1.,0.));
#3455=DIRECTION('',(0.,0.,-1.));
#3456=DIRECTION('center_axis',(0.5,0.866025403784439,0.));
#3457=DIRECTION('ref_axis',(0.866025403784439,-0.5,0.));
#3458=DIRECTION('',(0.,0.,-1.));
#3459=DIRECTION('center_axis',(-0.5,0.866025403784439,0.));
#3460=DIRECTION('ref_axis',(0.866025403784439,0.5,0.));
#3461=DIRECTION('',(0.,0.,-1.));
#3462=DIRECTION('center_axis',(-1.,6.40987562127854E-16,0.));
#3463=DIRECTION('ref_axis',(6.40987562127854E-16,1.,0.));
#3464=DIRECTION('',(0.,0.,-1.));
#3465=DIRECTION('center_axis',(-0.5,-0.866025403784439,0.));
#3466=DIRECTION('ref_axis',(-0.866025403784439,0.5,0.));
#3467=DIRECTION('center_axis',(1.06387651071382E-15,0.,-1.));
#3468=DIRECTION('ref_axis',(-1.,0.,-1.06387651071382E-15));
#3469=DIRECTION('',(-1.06387651071382E-15,0.,1.));
#3470=DIRECTION('center_axis',(-1.06387651071382E-15,0.,1.));
#3471=DIRECTION('ref_axis',(-1.,0.,-1.06387651071382E-15));
#3472=DIRECTION('center_axis',(1.06387651071382E-15,0.,-1.));
#3473=DIRECTION('ref_axis',(-1.,0.,-1.06387651071382E-15));
#3474=DIRECTION('center_axis',(1.06387651071382E-15,0.,-1.));
#3475=DIRECTION('ref_axis',(-1.,0.,-1.06387651071382E-15));
#3476=DIRECTION('axis',(0.,0.,1.));
#3477=DIRECTION('refdir',(1.,0.,0.));
#3478=DIRECTION('center_axis',(0.,0.,1.));
#3479=DIRECTION('ref_axis',(-1.,0.,0.));
#3480=DIRECTION('center_axis',(-1.06387651071382E-15,0.,1.));
#3481=DIRECTION('ref_axis',(-1.,0.,-1.06387651071382E-15));
#3482=DIRECTION('',(-0.73423251512767,-8.99175499481012E-17,-0.678898087881602));
#3483=DIRECTION('center_axis',(1.06387651071382E-15,0.,-1.));
#3484=DIRECTION('ref_axis',(-1.,0.,-1.06387651071382E-15));
#3485=DIRECTION('center_axis',(1.06387651071382E-15,0.,-1.));
#3486=DIRECTION('ref_axis',(-1.,0.,-1.05179023385541E-15));
#3487=DIRECTION('center_axis',(-1.06387651071382E-15,0.,1.));
#3488=DIRECTION('ref_axis',(1.,0.,1.06387651071382E-15));
#3489=DIRECTION('center_axis',(-1.22464679914735E-16,-1.,-1.30287296353373E-31));
#3490=DIRECTION('ref_axis',(1.,-1.22464679914735E-16,1.02257383847054E-15));
#3491=DIRECTION('center_axis',(1.06387651071382E-15,0.,-1.));
#3492=DIRECTION('ref_axis',(1.,0.,1.06387651071382E-15));
#3493=DIRECTION('center_axis',(-1.06387651071382E-15,0.,1.));
#3494=DIRECTION('ref_axis',(1.,0.,1.06387651071382E-15));
#3495=DIRECTION('',(-0.866025403784439,-0.5,-9.21344084767719E-16));
#3496=DIRECTION('',(-0.866025403784439,0.5,-9.21344084767719E-16));
#3497=DIRECTION('',(6.40987562127854E-16,1.,6.81931611007542E-31));
#3498=DIRECTION('',(0.866025403784439,0.5,9.21344084767719E-16));
#3499=DIRECTION('',(0.866025403784439,-0.5,9.21344084767719E-16));
#3500=DIRECTION('',(-1.60246890531964E-16,-1.,-1.70482902751885E-31));
#3501=DIRECTION('center_axis',(1.06387651071382E-15,0.,-1.));
#3502=DIRECTION('ref_axis',(-1.,0.,-1.06387651071382E-15));
#3503=DIRECTION('center_axis',(1.06387651071382E-15,0.,-1.));
#3504=DIRECTION('ref_axis',(1.,0.,1.06387651071382E-15));
#3505=DIRECTION('',(-1.06387651071382E-15,0.,1.));
#3506=DIRECTION('center_axis',(0.0435778713738291,-0.0754790873051733,-0.996194698091746));
#3507=DIRECTION('ref_axis',(-0.866025403784439,-0.5,-3.35810244624808E-17));
#3508=DIRECTION('',(0.,0.997141949694316,-0.0755508581011305));
#3509=DIRECTION('',(-0.866025403784439,-0.5,0.));
#3510=DIRECTION('',(-0.863550259614423,0.498570974847158,-0.0755508581011305));
#3511=DIRECTION('center_axis',(0.0871557427476581,-1.3966436767316E-17,
-0.996194698091746));
#3512=DIRECTION('ref_axis',(-1.60246890531964E-16,-1.,1.77292017095641E-32));
#3513=DIRECTION('',(-1.60246890531964E-16,-1.,0.));
#3514=DIRECTION('',(-0.863550259614423,-0.498570974847158,-0.0755508581011305));
#3515=DIRECTION('center_axis',(0.0435778713738291,0.0754790873051733,-0.996194698091746));
#3516=DIRECTION('ref_axis',(0.866025403784439,-0.5,3.35810244624808E-17));
#3517=DIRECTION('',(0.866025403784439,-0.5,0.));
#3518=DIRECTION('',(-1.59381164582915E-16,-0.997141949694316,-0.0755508581011305));
#3519=DIRECTION('center_axis',(-0.0435778713738291,0.0754790873051733,-0.996194698091746));
#3520=DIRECTION('ref_axis',(0.866025403784439,0.5,-3.35810244624808E-17));
#3521=DIRECTION('',(0.866025403784439,0.5,0.));
#3522=DIRECTION('',(0.863550259614423,-0.498570974847159,-0.0755508581011305));
#3523=DIRECTION('center_axis',(-0.0871557427476581,5.58657470692638E-17,
-0.996194698091746));
#3524=DIRECTION('ref_axis',(6.40987562127854E-16,1.,4.7015367027096E-32));
#3525=DIRECTION('',(6.40987562127854E-16,1.,0.));
#3526=DIRECTION('',(0.863550259614423,0.498570974847158,-0.0755508581011305));
#3527=DIRECTION('center_axis',(-0.0435778713738291,-0.0754790873051733,
-0.996194698091746));
#3528=DIRECTION('ref_axis',(-0.866025403784439,0.5,3.35810244624808E-17));
#3529=DIRECTION('',(-0.866025403784439,0.5,0.));
#3530=DIRECTION('center_axis',(0.5,-0.866025403784439,0.));
#3531=DIRECTION('ref_axis',(-0.866025403784439,-0.5,0.));
#3532=DIRECTION('',(0.,0.,-1.));
#3533=DIRECTION('',(0.,0.,-1.));
#3534=DIRECTION('center_axis',(1.,-1.60246890531964E-16,0.));
#3535=DIRECTION('ref_axis',(-1.60246890531964E-16,-1.,0.));
#3536=DIRECTION('',(0.,0.,-1.));
#3537=DIRECTION('center_axis',(0.5,0.866025403784439,0.));
#3538=DIRECTION('ref_axis',(0.866025403784439,-0.5,0.));
#3539=DIRECTION('',(0.,0.,-1.));
#3540=DIRECTION('center_axis',(-0.5,0.866025403784439,0.));
#3541=DIRECTION('ref_axis',(0.866025403784439,0.5,0.));
#3542=DIRECTION('',(0.,0.,-1.));
#3543=DIRECTION('center_axis',(-1.,6.40987562127854E-16,0.));
#3544=DIRECTION('ref_axis',(6.40987562127854E-16,1.,0.));
#3545=DIRECTION('',(0.,0.,-1.));
#3546=DIRECTION('center_axis',(-0.5,-0.866025403784439,0.));
#3547=DIRECTION('ref_axis',(-0.866025403784439,0.5,0.));
#3548=DIRECTION('center_axis',(1.06387651071382E-15,0.,-1.));
#3549=DIRECTION('ref_axis',(-1.,0.,-1.06387651071382E-15));
#3550=DIRECTION('',(-1.06387651071382E-15,0.,1.));
#3551=DIRECTION('center_axis',(-1.06387651071382E-15,0.,1.));
#3552=DIRECTION('ref_axis',(-1.,0.,-1.06387651071382E-15));
#3553=DIRECTION('center_axis',(1.06387651071382E-15,0.,-1.));
#3554=DIRECTION('ref_axis',(-1.,0.,-1.06387651071382E-15));
#3555=DIRECTION('center_axis',(1.06387651071382E-15,0.,-1.));
#3556=DIRECTION('ref_axis',(-1.,0.,-1.06387651071382E-15));
#3557=DIRECTION('axis',(0.,0.,1.));
#3558=DIRECTION('refdir',(1.,0.,0.));
#3559=DIRECTION('center_axis',(0.,0.,1.));
#3560=DIRECTION('ref_axis',(-1.,0.,0.));
#3561=DIRECTION('center_axis',(-1.06387651071382E-15,0.,1.));
#3562=DIRECTION('ref_axis',(-1.,0.,-1.06387651071382E-15));
#3563=DIRECTION('',(-0.73423251512767,-8.99175499481012E-17,-0.678898087881602));
#3564=DIRECTION('center_axis',(1.06387651071382E-15,0.,-1.));
#3565=DIRECTION('ref_axis',(-1.,0.,-1.06387651071382E-15));
#3566=DIRECTION('center_axis',(1.06387651071382E-15,0.,-1.));
#3567=DIRECTION('ref_axis',(-1.,0.,-1.05179023385541E-15));
#3568=DIRECTION('center_axis',(-1.06387651071382E-15,0.,1.));
#3569=DIRECTION('ref_axis',(1.,0.,1.06387651071382E-15));
#3570=DIRECTION('center_axis',(-1.22464679914735E-16,-1.,-1.30287296353373E-31));
#3571=DIRECTION('ref_axis',(1.,-1.22464679914735E-16,1.02257383847054E-15));
#3572=DIRECTION('center_axis',(1.06387651071382E-15,0.,-1.));
#3573=DIRECTION('ref_axis',(1.,0.,1.06387651071382E-15));
#3574=DIRECTION('center_axis',(-1.06387651071382E-15,0.,1.));
#3575=DIRECTION('ref_axis',(1.,0.,1.06387651071382E-15));
#3576=DIRECTION('',(-0.866025403784439,-0.5,-9.21344084767719E-16));
#3577=DIRECTION('',(-0.866025403784439,0.5,-9.21344084767719E-16));
#3578=DIRECTION('',(6.40987562127854E-16,1.,6.81931611007542E-31));
#3579=DIRECTION('',(0.866025403784439,0.5,9.21344084767719E-16));
#3580=DIRECTION('',(0.866025403784439,-0.5,9.21344084767719E-16));
#3581=DIRECTION('',(-1.60246890531964E-16,-1.,-1.70482902751885E-31));
#3582=DIRECTION('center_axis',(1.06387651071382E-15,0.,-1.));
#3583=DIRECTION('ref_axis',(-1.,0.,-1.06387651071382E-15));
#3584=DIRECTION('center_axis',(1.06387651071382E-15,0.,-1.));
#3585=DIRECTION('ref_axis',(1.,0.,1.06387651071382E-15));
#3586=DIRECTION('',(-1.06387651071382E-15,0.,1.));
#3587=DIRECTION('center_axis',(0.0435778713738291,-0.0754790873051733,-0.996194698091746));
#3588=DIRECTION('ref_axis',(-0.866025403784439,-0.5,-3.35810244624808E-17));
#3589=DIRECTION('',(0.,0.997141949694316,-0.0755508581011305));
#3590=DIRECTION('',(-0.866025403784439,-0.5,0.));
#3591=DIRECTION('',(-0.863550259614423,0.498570974847158,-0.0755508581011305));
#3592=DIRECTION('center_axis',(0.0871557427476581,-1.3966436767316E-17,
-0.996194698091746));
#3593=DIRECTION('ref_axis',(-1.60246890531964E-16,-1.,1.77292017095641E-32));
#3594=DIRECTION('',(-1.60246890531964E-16,-1.,0.));
#3595=DIRECTION('',(-0.863550259614423,-0.498570974847158,-0.0755508581011305));
#3596=DIRECTION('center_axis',(0.0435778713738291,0.0754790873051733,-0.996194698091746));
#3597=DIRECTION('ref_axis',(0.866025403784439,-0.5,3.35810244624808E-17));
#3598=DIRECTION('',(0.866025403784439,-0.5,0.));
#3599=DIRECTION('',(-1.59381164582915E-16,-0.997141949694316,-0.0755508581011305));
#3600=DIRECTION('center_axis',(-0.0435778713738291,0.0754790873051733,-0.996194698091746));
#3601=DIRECTION('ref_axis',(0.866025403784439,0.5,-3.35810244624808E-17));
#3602=DIRECTION('',(0.866025403784439,0.5,0.));
#3603=DIRECTION('',(0.863550259614423,-0.498570974847159,-0.0755508581011305));
#3604=DIRECTION('center_axis',(-0.0871557427476581,5.58657470692638E-17,
-0.996194698091746));
#3605=DIRECTION('ref_axis',(6.40987562127854E-16,1.,4.7015367027096E-32));
#3606=DIRECTION('',(6.40987562127854E-16,1.,0.));
#3607=DIRECTION('',(0.863550259614423,0.498570974847158,-0.0755508581011305));
#3608=DIRECTION('center_axis',(-0.0435778713738291,-0.0754790873051733,
-0.996194698091746));
#3609=DIRECTION('ref_axis',(-0.866025403784439,0.5,3.35810244624808E-17));
#3610=DIRECTION('',(-0.866025403784439,0.5,0.));
#3611=DIRECTION('center_axis',(0.5,-0.866025403784439,0.));
#3612=DIRECTION('ref_axis',(-0.866025403784439,-0.5,0.));
#3613=DIRECTION('',(0.,0.,-1.));
#3614=DIRECTION('',(0.,0.,-1.));
#3615=DIRECTION('center_axis',(1.,-1.60246890531964E-16,0.));
#3616=DIRECTION('ref_axis',(-1.60246890531964E-16,-1.,0.));
#3617=DIRECTION('',(0.,0.,-1.));
#3618=DIRECTION('center_axis',(0.5,0.866025403784439,0.));
#3619=DIRECTION('ref_axis',(0.866025403784439,-0.5,0.));
#3620=DIRECTION('',(0.,0.,-1.));
#3621=DIRECTION('center_axis',(-0.5,0.866025403784439,0.));
#3622=DIRECTION('ref_axis',(0.866025403784439,0.5,0.));
#3623=DIRECTION('',(0.,0.,-1.));
#3624=DIRECTION('center_axis',(-1.,6.40987562127854E-16,0.));
#3625=DIRECTION('ref_axis',(6.40987562127854E-16,1.,0.));
#3626=DIRECTION('',(0.,0.,-1.));
#3627=DIRECTION('center_axis',(-0.5,-0.866025403784439,0.));
#3628=DIRECTION('ref_axis',(-0.866025403784439,0.5,0.));
#3629=DIRECTION('center_axis',(1.06387651071382E-15,0.,-1.));
#3630=DIRECTION('ref_axis',(-1.,0.,-1.06387651071382E-15));
#3631=DIRECTION('',(-1.06387651071382E-15,0.,1.));
#3632=DIRECTION('center_axis',(-1.06387651071382E-15,0.,1.));
#3633=DIRECTION('ref_axis',(-1.,0.,-1.06387651071382E-15));
#3634=DIRECTION('center_axis',(1.06387651071382E-15,0.,-1.));
#3635=DIRECTION('ref_axis',(-1.,0.,-1.06387651071382E-15));
#3636=DIRECTION('center_axis',(1.06387651071382E-15,0.,-1.));
#3637=DIRECTION('ref_axis',(-1.,0.,-1.06387651071382E-15));
#3638=DIRECTION('axis',(0.,0.,1.));
#3639=DIRECTION('refdir',(1.,0.,0.));
#3640=DIRECTION('center_axis',(0.,0.,-1.));
#3641=DIRECTION('ref_axis',(-1.,0.,0.));
#3642=DIRECTION('center_axis',(0.,0.,1.));
#3643=DIRECTION('ref_axis',(-1.,0.,0.));
#3644=DIRECTION('',(0.707106781186547,-8.65956056235492E-17,-0.707106781186548));
#3645=DIRECTION('center_axis',(0.,0.,-1.));
#3646=DIRECTION('ref_axis',(-1.,0.,0.));
#3647=DIRECTION('center_axis',(0.,0.,-1.));
#3648=DIRECTION('ref_axis',(0.,1.,0.));
#3649=DIRECTION('',(1.,0.,0.));
#3650=DIRECTION('',(0.,-1.,0.));
#3651=DIRECTION('',(1.,0.,0.));
#3652=DIRECTION('',(0.,-1.,0.));
#3653=DIRECTION('center_axis',(0.,0.,-1.));
#3654=DIRECTION('ref_axis',(-1.,0.,0.));
#3655=DIRECTION('center_axis',(0.,0.,-1.));
#3656=DIRECTION('ref_axis',(-1.,0.,0.));
#3657=DIRECTION('center_axis',(0.,0.,-1.));
#3658=DIRECTION('ref_axis',(-1.,0.,0.));
#3659=DIRECTION('center_axis',(0.,0.,-1.));
#3660=DIRECTION('ref_axis',(-1.,0.,0.));
#3661=DIRECTION('center_axis',(0.,0.,-1.));
#3662=DIRECTION('ref_axis',(-1.,0.,0.));
#3663=DIRECTION('center_axis',(0.,0.,1.));
#3664=DIRECTION('ref_axis',(-1.,0.,0.));
#3665=DIRECTION('',(0.,0.,-1.));
#3666=DIRECTION('center_axis',(0.,0.,-1.));
#3667=DIRECTION('ref_axis',(-1.,0.,0.));
#3668=DIRECTION('center_axis',(0.,0.,1.));
#3669=DIRECTION('ref_axis',(-1.,0.,0.));
#3670=DIRECTION('',(0.707106781186547,-8.65956056235492E-17,-0.707106781186548));
#3671=DIRECTION('center_axis',(0.,0.,-1.));
#3672=DIRECTION('ref_axis',(-1.,0.,0.));
#3673=DIRECTION('center_axis',(0.,0.,1.));
#3674=DIRECTION('ref_axis',(-1.,0.,0.));
#3675=DIRECTION('',(0.,0.,-1.));
#3676=DIRECTION('center_axis',(0.,0.,-1.));
#3677=DIRECTION('ref_axis',(-1.,0.,0.));
#3678=DIRECTION('center_axis',(0.,0.,1.));
#3679=DIRECTION('ref_axis',(-1.,0.,0.));
#3680=DIRECTION('',(0.707106781186548,-8.65956056235494E-17,-0.707106781186547));
#3681=DIRECTION('center_axis',(0.,0.,-1.));
#3682=DIRECTION('ref_axis',(-1.,0.,0.));
#3683=DIRECTION('center_axis',(0.,0.,1.));
#3684=DIRECTION('ref_axis',(-1.,0.,0.));
#3685=DIRECTION('',(0.,0.,-1.));
#3686=DIRECTION('center_axis',(0.,0.,-1.));
#3687=DIRECTION('ref_axis',(-1.,0.,0.));
#3688=DIRECTION('center_axis',(0.,0.,1.));
#3689=DIRECTION('ref_axis',(-1.,0.,0.));
#3690=DIRECTION('',(0.707106781186549,-8.65956056235495E-17,-0.707106781186546));
#3691=DIRECTION('center_axis',(0.,0.,-1.));
#3692=DIRECTION('ref_axis',(-1.,0.,0.));
#3693=DIRECTION('center_axis',(0.,0.,1.));
#3694=DIRECTION('ref_axis',(-1.,0.,0.));
#3695=DIRECTION('',(0.,0.,-1.));
#3696=DIRECTION('center_axis',(0.,0.,-1.));
#3697=DIRECTION('ref_axis',(-1.,0.,0.));
#3698=DIRECTION('center_axis',(0.,0.,1.));
#3699=DIRECTION('ref_axis',(-1.,0.,0.));
#3700=DIRECTION('',(0.707106781186547,-8.65956056235492E-17,-0.707106781186548));
#3701=DIRECTION('center_axis',(0.,0.,-1.));
#3702=DIRECTION('ref_axis',(-1.,0.,0.));
#3703=DIRECTION('center_axis',(0.,0.,1.));
#3704=DIRECTION('ref_axis',(-1.,0.,0.));
#3705=DIRECTION('',(0.,0.,-1.));
#3706=DIRECTION('center_axis',(0.,0.,-1.));
#3707=DIRECTION('ref_axis',(-1.,0.,0.));
#3708=DIRECTION('center_axis',(0.,0.,-1.));
#3709=DIRECTION('ref_axis',(-1.,0.,0.));
#3710=DIRECTION('',(0.,0.,-1.));
#3711=DIRECTION('center_axis',(0.,0.,-1.));
#3712=DIRECTION('ref_axis',(-1.,0.,0.));
#3713=DIRECTION('center_axis',(0.,0.,1.));
#3714=DIRECTION('ref_axis',(-1.,0.,0.));
#3715=DIRECTION('center_axis',(0.,0.,-1.));
#3716=DIRECTION('ref_axis',(-1.,0.,0.));
#3717=DIRECTION('center_axis',(0.,0.,-1.));
#3718=DIRECTION('ref_axis',(-1.,0.,0.));
#3719=DIRECTION('',(0.,0.,-1.));
#3720=DIRECTION('center_axis',(0.,0.,-1.));
#3721=DIRECTION('ref_axis',(-1.,0.,0.));
#3722=DIRECTION('center_axis',(0.,0.,1.));
#3723=DIRECTION('ref_axis',(-1.,0.,0.));
#3724=DIRECTION('center_axis',(0.,0.,-1.));
#3725=DIRECTION('ref_axis',(-1.,0.,0.));
#3726=DIRECTION('center_axis',(0.,0.,-1.));
#3727=DIRECTION('ref_axis',(-1.,0.,0.));
#3728=DIRECTION('',(0.,0.,-1.));
#3729=DIRECTION('center_axis',(0.,0.,-1.));
#3730=DIRECTION('ref_axis',(-1.,0.,0.));
#3731=DIRECTION('center_axis',(0.,0.,1.));
#3732=DIRECTION('ref_axis',(-1.,0.,0.));
#3733=DIRECTION('center_axis',(0.,0.,-1.));
#3734=DIRECTION('ref_axis',(-1.,0.,0.));
#3735=DIRECTION('center_axis',(0.,0.,-1.));
#3736=DIRECTION('ref_axis',(-1.,0.,0.));
#3737=DIRECTION('',(0.,0.,-1.));
#3738=DIRECTION('center_axis',(0.,0.,-1.));
#3739=DIRECTION('ref_axis',(-1.,0.,0.));
#3740=DIRECTION('center_axis',(0.,0.,1.));
#3741=DIRECTION('ref_axis',(-1.,0.,0.));
#3742=DIRECTION('center_axis',(0.,0.,-1.));
#3743=DIRECTION('ref_axis',(-1.,0.,0.));
#3744=DIRECTION('center_axis',(0.,0.,-1.));
#3745=DIRECTION('ref_axis',(-1.,0.,0.));
#3746=DIRECTION('',(0.,0.,-1.));
#3747=DIRECTION('center_axis',(0.,0.,-1.));
#3748=DIRECTION('ref_axis',(-1.,0.,0.));
#3749=DIRECTION('center_axis',(0.,0.,1.));
#3750=DIRECTION('ref_axis',(-1.,0.,0.));
#3751=DIRECTION('center_axis',(0.,1.,0.));
#3752=DIRECTION('ref_axis',(0.,0.,1.));
#3753=DIRECTION('',(-1.,0.,0.));
#3754=DIRECTION('',(0.,0.,-1.));
#3755=DIRECTION('',(1.,0.,0.));
#3756=DIRECTION('',(0.,0.,1.));
#3757=DIRECTION('center_axis',(-1.,0.,0.));
#3758=DIRECTION('ref_axis',(0.,1.,1.18388150812306E-15));
#3759=DIRECTION('center_axis',(-1.,0.,0.));
#3760=DIRECTION('ref_axis',(0.,-0.0407335971034729,0.999170042618879));
#3761=DIRECTION('',(1.,0.,0.));
#3762=DIRECTION('center_axis',(1.,0.,0.));
#3763=DIRECTION('ref_axis',(0.,-0.0407335971034729,0.999170042618879));
#3764=DIRECTION('center_axis',(0.,1.,0.));
#3765=DIRECTION('ref_axis',(0.,0.,1.));
#3766=DIRECTION('',(0.,0.,-1.));
#3767=DIRECTION('',(0.,0.,1.));
#3768=DIRECTION('center_axis',(0.,0.706957380091336,-0.707256150722208));
#3769=DIRECTION('ref_axis',(0.,0.707256150722208,0.706957380091336));
#3770=DIRECTION('',(1.,0.,0.));
#3771=DIRECTION('',(0.,-0.707256150722208,-0.706957380091336));
#3772=DIRECTION('',(0.,0.707256150722208,0.706957380091336));
#3773=DIRECTION('center_axis',(1.,0.,0.));
#3774=DIRECTION('ref_axis',(0.,1.,0.));
#3775=DIRECTION('',(0.,0.707256150722208,-0.706957380091336));
#3776=DIRECTION('',(0.,0.,-1.));
#3777=DIRECTION('center_axis',(1.,0.,0.));
#3778=DIRECTION('ref_axis',(0.,0.0407335971034729,0.999170042618879));
#3779=DIRECTION('',(0.,0.,-1.));
#3780=DIRECTION('',(0.,-1.,0.));
#3781=DIRECTION('center_axis',(0.,1.,0.));
#3782=DIRECTION('ref_axis',(0.,0.,1.));
#3783=DIRECTION('',(-1.,0.,0.));
#3784=DIRECTION('',(0.,0.,1.));
#3785=DIRECTION('',(1.,0.,0.));
#3786=DIRECTION('center_axis',(1.,0.,0.));
#3787=DIRECTION('ref_axis',(0.,-1.,1.18388150812306E-15));
#3788=DIRECTION('center_axis',(-1.,0.,0.));
#3789=DIRECTION('ref_axis',(0.,0.0407335971034729,0.999170042618879));
#3790=DIRECTION('',(1.,0.,0.));
#3791=DIRECTION('center_axis',(0.,1.,0.));
#3792=DIRECTION('ref_axis',(0.,0.,1.));
#3793=DIRECTION('',(0.,0.,1.));
#3794=DIRECTION('center_axis',(0.,0.,1.));
#3795=DIRECTION('ref_axis',(0.,-1.,0.));
#3796=DIRECTION('',(0.,-1.,0.));
#3797=DIRECTION('',(1.,0.,0.));
#3798=DIRECTION('center_axis',(0.,0.706957380091336,0.707256150722208));
#3799=DIRECTION('ref_axis',(0.,-0.707256150722208,0.706957380091336));
#3800=DIRECTION('',(0.,-0.707256150722208,0.706957380091336));
#3801=DIRECTION('center_axis',(1.,0.,0.));
#3802=DIRECTION('ref_axis',(0.,1.,0.));
#3803=DIRECTION('axis',(0.,0.,1.));
#3804=DIRECTION('refdir',(1.,0.,0.));
#3805=DIRECTION('center_axis',(0.,0.,-1.));
#3806=DIRECTION('ref_axis',(-1.,0.,0.));
#3807=DIRECTION('center_axis',(0.,0.,-1.));
#3808=DIRECTION('ref_axis',(-1.,0.,0.));
#3809=DIRECTION('',(0.,0.,-1.));
#3810=DIRECTION('center_axis',(0.,0.,-1.));
#3811=DIRECTION('ref_axis',(-1.,0.,0.));
#3812=DIRECTION('center_axis',(0.,0.,1.));
#3813=DIRECTION('ref_axis',(-1.,0.,0.));
#3814=DIRECTION('center_axis',(0.,0.,-1.));
#3815=DIRECTION('ref_axis',(-1.,0.,0.));
#3816=DIRECTION('center_axis',(0.,0.,-1.));
#3817=DIRECTION('ref_axis',(-1.,0.,0.));
#3818=DIRECTION('',(0.,0.,-1.));
#3819=DIRECTION('center_axis',(0.,0.,-1.));
#3820=DIRECTION('ref_axis',(-1.,0.,0.));
#3821=DIRECTION('center_axis',(0.,0.,1.));
#3822=DIRECTION('ref_axis',(-1.,0.,0.));
#3823=DIRECTION('center_axis',(0.,0.,-1.));
#3824=DIRECTION('ref_axis',(-1.,0.,0.));
#3825=DIRECTION('center_axis',(0.,0.,-1.));
#3826=DIRECTION('ref_axis',(-1.,0.,0.));
#3827=DIRECTION('',(0.,0.,-1.));
#3828=DIRECTION('center_axis',(0.,0.,-1.));
#3829=DIRECTION('ref_axis',(-1.,0.,0.));
#3830=DIRECTION('center_axis',(0.,0.,1.));
#3831=DIRECTION('ref_axis',(-1.,0.,0.));
#3832=DIRECTION('center_axis',(0.,0.,-1.));
#3833=DIRECTION('ref_axis',(-1.,0.,0.));
#3834=DIRECTION('center_axis',(0.,0.,-1.));
#3835=DIRECTION('ref_axis',(-1.,0.,0.));
#3836=DIRECTION('',(0.,0.,-1.));
#3837=DIRECTION('center_axis',(0.,0.,-1.));
#3838=DIRECTION('ref_axis',(-1.,0.,0.));
#3839=DIRECTION('center_axis',(0.,0.,1.));
#3840=DIRECTION('ref_axis',(-1.,0.,0.));
#3841=DIRECTION('center_axis',(-1.,0.,0.));
#3842=DIRECTION('ref_axis',(0.,0.,1.));
#3843=DIRECTION('',(0.,-1.,0.));
#3844=DIRECTION('',(0.,0.,-1.));
#3845=DIRECTION('',(0.,-1.,0.));
#3846=DIRECTION('',(0.,0.,1.));
#3847=DIRECTION('',(0.,1.,0.));
#3848=DIRECTION('',(0.,0.723499719481454,-0.690324674273097));
#3849=DIRECTION('',(0.,1.,0.));
#3850=DIRECTION('',(0.,0.723499719481453,0.690324674273098));
#3851=DIRECTION('',(0.,1.,0.));
#3852=DIRECTION('',(0.,0.,-1.));
#3853=DIRECTION('',(0.,-1.,0.));
#3854=DIRECTION('',(0.,0.,1.));
#3855=DIRECTION('center_axis',(0.,1.,0.));
#3856=DIRECTION('ref_axis',(0.,0.,1.));
#3857=DIRECTION('',(1.,0.,0.));
#3858=DIRECTION('',(0.,0.,1.));
#3859=DIRECTION('',(1.,0.,0.));
#3860=DIRECTION('center_axis',(0.,0.,-1.));
#3861=DIRECTION('ref_axis',(0.,1.,0.));
#3862=DIRECTION('',(0.,1.,0.));
#3863=DIRECTION('',(1.,0.,0.));
#3864=DIRECTION('center_axis',(0.,-1.,0.));
#3865=DIRECTION('ref_axis',(0.,0.,-1.));
#3866=DIRECTION('',(0.,0.,-1.));
#3867=DIRECTION('',(1.,0.,0.));
#3868=DIRECTION('center_axis',(0.,0.,1.));
#3869=DIRECTION('ref_axis',(0.,-1.,0.));
#3870=DIRECTION('',(0.,-1.,0.));
#3871=DIRECTION('',(1.,0.,0.));
#3872=DIRECTION('center_axis',(0.,0.690324674273097,0.723499719481454));
#3873=DIRECTION('ref_axis',(0.,-0.723499719481454,0.690324674273097));
#3874=DIRECTION('',(0.,-0.723499719481454,0.690324674273097));
#3875=DIRECTION('',(1.,0.,0.));
#3876=DIRECTION('center_axis',(0.,0.,1.));
#3877=DIRECTION('ref_axis',(0.,-1.,0.));
#3878=DIRECTION('',(0.,-1.,0.));
#3879=DIRECTION('',(1.,0.,0.));
#3880=DIRECTION('center_axis',(0.,-0.690324674273098,0.723499719481453));
#3881=DIRECTION('ref_axis',(0.,-0.723499719481453,-0.690324674273098));
#3882=DIRECTION('',(0.,-0.723499719481453,-0.690324674273098));
#3883=DIRECTION('',(1.,0.,0.));
#3884=DIRECTION('center_axis',(0.,0.,1.));
#3885=DIRECTION('ref_axis',(0.,-1.,0.));
#3886=DIRECTION('',(0.,-1.,0.));
#3887=DIRECTION('',(1.,0.,0.));
#3888=DIRECTION('center_axis',(0.,1.,0.));
#3889=DIRECTION('ref_axis',(0.,0.,1.));
#3890=DIRECTION('',(0.,0.,1.));
#3891=DIRECTION('',(1.,0.,0.));
#3892=DIRECTION('center_axis',(0.,0.,-1.));
#3893=DIRECTION('ref_axis',(0.,1.,0.));
#3894=DIRECTION('',(0.,1.,0.));
#3895=DIRECTION('',(1.,0.,0.));
#3896=DIRECTION('center_axis',(0.,-1.,0.));
#3897=DIRECTION('ref_axis',(0.,0.,-1.));
#3898=DIRECTION('',(0.,0.,-1.));
#3899=DIRECTION('',(1.,0.,0.));
#3900=DIRECTION('center_axis',(0.,0.,-1.));
#3901=DIRECTION('ref_axis',(0.,1.,0.));
#3902=DIRECTION('',(0.,1.,0.));
#3903=DIRECTION('center_axis',(1.,0.,0.));
#3904=DIRECTION('ref_axis',(0.,0.,-1.));
#3905=DIRECTION('axis',(0.,0.,1.));
#3906=DIRECTION('refdir',(1.,0.,0.));
#3907=DIRECTION('center_axis',(-1.,0.,0.));
#3908=DIRECTION('ref_axis',(0.,1.,0.));
#3909=DIRECTION('center_axis',(1.,0.,0.));
#3910=DIRECTION('ref_axis',(0.,1.,0.));
#3911=DIRECTION('',(-1.,0.,0.));
#3912=DIRECTION('center_axis',(-1.,0.,0.));
#3913=DIRECTION('ref_axis',(0.,1.,0.));
#3914=DIRECTION('center_axis',(-1.,0.,0.));
#3915=DIRECTION('ref_axis',(0.,1.,0.));
#3916=DIRECTION('center_axis',(1.,0.,0.));
#3917=DIRECTION('ref_axis',(0.,1.,0.));
#3918=DIRECTION('',(-1.,0.,0.));
#3919=DIRECTION('center_axis',(-1.,0.,0.));
#3920=DIRECTION('ref_axis',(0.,1.,0.));
#3921=DIRECTION('center_axis',(0.,0.,-1.));
#3922=DIRECTION('ref_axis',(0.,-1.,0.));
#3923=DIRECTION('',(0.,-1.,0.));
#3924=DIRECTION('',(-1.,0.,0.));
#3925=DIRECTION('',(0.,-1.,0.));
#3926=DIRECTION('',(-1.,0.,0.));
#3927=DIRECTION('center_axis',(0.,-1.,0.));
#3928=DIRECTION('ref_axis',(0.,0.,1.));
#3929=DIRECTION('',(0.,0.,1.));
#3930=DIRECTION('',(-1.,0.,0.));
#3931=DIRECTION('',(0.,0.,1.));
#3932=DIRECTION('center_axis',(0.,0.,1.));
#3933=DIRECTION('ref_axis',(0.,1.,0.));
#3934=DIRECTION('',(0.,1.,0.));
#3935=DIRECTION('',(-1.,0.,0.));
#3936=DIRECTION('',(0.,1.,0.));
#3937=DIRECTION('center_axis',(0.,1.,0.));
#3938=DIRECTION('ref_axis',(0.,0.,-1.));
#3939=DIRECTION('',(0.,0.,-1.));
#3940=DIRECTION('',(-1.,0.,0.));
#3941=DIRECTION('',(0.,0.,-1.));
#3942=DIRECTION('center_axis',(0.,0.,1.));
#3943=DIRECTION('ref_axis',(0.,1.,0.));
#3944=DIRECTION('',(0.,1.,0.));
#3945=DIRECTION('',(-1.,0.,0.));
#3946=DIRECTION('',(0.,1.,0.));
#3947=DIRECTION('center_axis',(0.,-1.,1.24327477962315E-16));
#3948=DIRECTION('ref_axis',(0.,1.24327477962315E-16,1.));
#3949=DIRECTION('',(0.,1.24327477962315E-16,1.));
#3950=DIRECTION('',(-1.,0.,0.));
#3951=DIRECTION('',(0.,1.24327477962315E-16,1.));
#3952=DIRECTION('center_axis',(0.,0.,1.));
#3953=DIRECTION('ref_axis',(0.,1.,0.));
#3954=DIRECTION('',(0.,1.,0.));
#3955=DIRECTION('',(-1.,0.,0.));
#3956=DIRECTION('',(0.,1.,0.));
#3957=DIRECTION('center_axis',(0.,1.,0.));
#3958=DIRECTION('ref_axis',(0.,0.,-1.));
#3959=DIRECTION('',(0.,0.,-1.));
#3960=DIRECTION('',(0.,0.,-1.));
#3961=DIRECTION('center_axis',(1.,0.,0.));
#3962=DIRECTION('ref_axis',(0.,0.,-1.));
#3963=DIRECTION('center_axis',(1.,0.,0.));
#3964=DIRECTION('ref_axis',(0.,1.,0.));
#3965=DIRECTION('axis',(0.,0.,1.));
#3966=DIRECTION('refdir',(1.,0.,0.));
#3967=DIRECTION('center_axis',(-1.,0.,0.));
#3968=DIRECTION('ref_axis',(0.,1.,0.));
#3969=DIRECTION('center_axis',(-1.,0.,0.));
#3970=DIRECTION('ref_axis',(0.,1.,0.));
#3971=DIRECTION('',(-1.,0.,0.));
#3972=DIRECTION('center_axis',(1.,0.,0.));
#3973=DIRECTION('ref_axis',(0.,1.,0.));
#3974=DIRECTION('center_axis',(-1.,0.,0.));
#3975=DIRECTION('ref_axis',(0.,1.,0.));
#3976=DIRECTION('center_axis',(-1.,0.,0.));
#3977=DIRECTION('ref_axis',(0.,1.,0.));
#3978=DIRECTION('',(-1.,0.,0.));
#3979=DIRECTION('center_axis',(1.,0.,0.));
#3980=DIRECTION('ref_axis',(0.,1.,0.));
#3981=DIRECTION('center_axis',(0.,1.,0.));
#3982=DIRECTION('ref_axis',(0.,0.,1.));
#3983=DIRECTION('',(0.,0.,1.));
#3984=DIRECTION('',(1.,0.,0.));
#3985=DIRECTION('',(0.,0.,1.));
#3986=DIRECTION('',(1.,0.,0.));
#3987=DIRECTION('center_axis',(0.,0.,-1.));
#3988=DIRECTION('ref_axis',(0.,1.,0.));
#3989=DIRECTION('',(0.,1.,0.));
#3990=DIRECTION('',(0.,1.,0.));
#3991=DIRECTION('',(1.,0.,0.));
#3992=DIRECTION('center_axis',(0.,-1.,0.));
#3993=DIRECTION('ref_axis',(0.,0.,-1.));
#3994=DIRECTION('',(0.,0.,-1.));
#3995=DIRECTION('',(0.,0.,-1.));
#3996=DIRECTION('',(1.,0.,0.));
#3997=DIRECTION('center_axis',(0.,0.,-1.));
#3998=DIRECTION('ref_axis',(0.,1.,0.));
#3999=DIRECTION('',(0.,1.,0.));
#4000=DIRECTION('',(0.,1.,0.));
#4001=DIRECTION('',(1.,0.,0.));
#4002=DIRECTION('center_axis',(0.,1.,0.));
#4003=DIRECTION('ref_axis',(0.,0.,1.));
#4004=DIRECTION('',(0.,0.,1.));
#4005=DIRECTION('',(0.,0.,1.));
#4006=DIRECTION('',(1.,0.,0.));
#4007=DIRECTION('center_axis',(0.,0.,-1.));
#4008=DIRECTION('ref_axis',(0.,1.,0.));
#4009=DIRECTION('',(0.,1.,0.));
#4010=DIRECTION('',(0.,1.,0.));
#4011=DIRECTION('',(1.,0.,0.));
#4012=DIRECTION('center_axis',(0.,-1.,0.));
#4013=DIRECTION('ref_axis',(0.,0.,-1.));
#4014=DIRECTION('',(0.,0.,-1.));
#4015=DIRECTION('',(0.,0.,-1.));
#4016=DIRECTION('',(1.,0.,0.));
#4017=DIRECTION('center_axis',(0.,0.,1.));
#4018=DIRECTION('ref_axis',(0.,-1.,0.));
#4019=DIRECTION('',(0.,-1.,0.));
#4020=DIRECTION('',(0.,-1.,0.));
#4021=DIRECTION('center_axis',(1.,0.,0.));
#4022=DIRECTION('ref_axis',(0.,0.,-1.));
#4023=DIRECTION('center_axis',(1.,0.,0.));
#4024=DIRECTION('ref_axis',(0.,1.,0.));
#4025=DIRECTION('axis',(0.,0.,1.));
#4026=DIRECTION('refdir',(1.,0.,0.));
#4027=DIRECTION('center_axis',(-1.,0.,0.));
#4028=DIRECTION('ref_axis',(0.,1.,0.));
#4029=DIRECTION('center_axis',(1.,0.,0.));
#4030=DIRECTION('ref_axis',(0.,1.,0.));
#4031=DIRECTION('',(-1.,0.,0.));
#4032=DIRECTION('center_axis',(-1.,0.,0.));
#4033=DIRECTION('ref_axis',(0.,1.,0.));
#4034=DIRECTION('center_axis',(-1.,0.,0.));
#4035=DIRECTION('ref_axis',(0.,1.,0.));
#4036=DIRECTION('center_axis',(1.,0.,0.));
#4037=DIRECTION('ref_axis',(0.,1.,0.));
#4038=DIRECTION('',(-1.,0.,0.));
#4039=DIRECTION('center_axis',(-1.,0.,0.));
#4040=DIRECTION('ref_axis',(0.,1.,0.));
#4041=DIRECTION('center_axis',(0.,-1.,0.));
#4042=DIRECTION('ref_axis',(0.,0.,1.));
#4043=DIRECTION('',(0.,0.,1.));
#4044=DIRECTION('',(-1.,0.,0.));
#4045=DIRECTION('',(0.,0.,1.));
#4046=DIRECTION('',(-1.,0.,0.));
#4047=DIRECTION('center_axis',(0.,0.,1.));
#4048=DIRECTION('ref_axis',(0.,1.,0.));
#4049=DIRECTION('',(0.,1.,0.));
#4050=DIRECTION('',(-1.,0.,0.));
#4051=DIRECTION('',(0.,1.,0.));
#4052=DIRECTION('center_axis',(0.,1.,0.));
#4053=DIRECTION('ref_axis',(0.,0.,-1.));
#4054=DIRECTION('',(0.,0.,-1.));
#4055=DIRECTION('',(-1.,0.,0.));
#4056=DIRECTION('',(0.,0.,-1.));
#4057=DIRECTION('center_axis',(0.,0.,1.));
#4058=DIRECTION('ref_axis',(0.,1.,0.));
#4059=DIRECTION('',(0.,1.,0.));
#4060=DIRECTION('',(-1.,0.,0.));
#4061=DIRECTION('',(0.,1.,0.));
#4062=DIRECTION('center_axis',(0.,-1.,0.));
#4063=DIRECTION('ref_axis',(0.,0.,1.));
#4064=DIRECTION('',(0.,0.,1.));
#4065=DIRECTION('',(-1.,0.,0.));
#4066=DIRECTION('',(0.,0.,1.));
#4067=DIRECTION('center_axis',(0.,0.,1.));
#4068=DIRECTION('ref_axis',(0.,1.,0.));
#4069=DIRECTION('',(0.,1.,0.));
#4070=DIRECTION('',(-1.,0.,0.));
#4071=DIRECTION('',(0.,1.,0.));
#4072=DIRECTION('center_axis',(0.,1.,0.));
#4073=DIRECTION('ref_axis',(0.,0.,-1.));
#4074=DIRECTION('',(0.,0.,-1.));
#4075=DIRECTION('',(-1.,0.,0.));
#4076=DIRECTION('',(0.,0.,-1.));
#4077=DIRECTION('center_axis',(0.,0.,-1.));
#4078=DIRECTION('ref_axis',(0.,-1.,0.));
#4079=DIRECTION('',(0.,-1.,0.));
#4080=DIRECTION('',(0.,-1.,0.));
#4081=DIRECTION('center_axis',(1.,0.,0.));
#4082=DIRECTION('ref_axis',(0.,0.,-1.));
#4083=DIRECTION('center_axis',(1.,0.,0.));
#4084=DIRECTION('ref_axis',(0.,1.,0.));
#4085=DIRECTION('axis',(0.,0.,1.));
#4086=DIRECTION('refdir',(1.,0.,0.));
#4087=DIRECTION('center_axis',(-1.,0.,0.));
#4088=DIRECTION('ref_axis',(0.,1.,0.));
#4089=DIRECTION('center_axis',(-1.,0.,0.));
#4090=DIRECTION('ref_axis',(0.,1.,0.));
#4091=DIRECTION('',(-1.,0.,0.));
#4092=DIRECTION('center_axis',(1.,0.,0.));
#4093=DIRECTION('ref_axis',(0.,1.,0.));
#4094=DIRECTION('center_axis',(-1.,0.,0.));
#4095=DIRECTION('ref_axis',(0.,1.,0.));
#4096=DIRECTION('center_axis',(-1.,0.,0.));
#4097=DIRECTION('ref_axis',(0.,1.,0.));
#4098=DIRECTION('',(-1.,0.,0.));
#4099=DIRECTION('center_axis',(1.,0.,0.));
#4100=DIRECTION('ref_axis',(0.,1.,0.));
#4101=DIRECTION('center_axis',(0.,0.,1.));
#4102=DIRECTION('ref_axis',(0.,-1.,0.));
#4103=DIRECTION('',(0.,-1.,0.));
#4104=DIRECTION('',(1.,0.,0.));
#4105=DIRECTION('',(0.,-1.,0.));
#4106=DIRECTION('',(1.,0.,0.));
#4107=DIRECTION('center_axis',(0.,1.,0.));
#4108=DIRECTION('ref_axis',(0.,0.,1.));
#4109=DIRECTION('',(0.,0.,1.));
#4110=DIRECTION('',(0.,0.,1.));
#4111=DIRECTION('',(1.,0.,0.));
#4112=DIRECTION('center_axis',(0.,0.,-1.));
#4113=DIRECTION('ref_axis',(0.,1.,0.));
#4114=DIRECTION('',(0.,1.,0.));
#4115=DIRECTION('',(0.,1.,0.));
#4116=DIRECTION('',(1.,0.,0.));
#4117=DIRECTION('center_axis',(0.,-1.,0.));
#4118=DIRECTION('ref_axis',(0.,0.,-1.));
#4119=DIRECTION('',(0.,0.,-1.));
#4120=DIRECTION('',(0.,0.,-1.));
#4121=DIRECTION('',(1.,0.,0.));
#4122=DIRECTION('center_axis',(0.,0.,-1.));
#4123=DIRECTION('ref_axis',(0.,1.,0.));
#4124=DIRECTION('',(0.,1.,0.));
#4125=DIRECTION('',(0.,1.,0.));
#4126=DIRECTION('',(1.,0.,0.));
#4127=DIRECTION('center_axis',(0.,1.,-1.24327477962315E-16));
#4128=DIRECTION('ref_axis',(0.,1.24327477962315E-16,1.));
#4129=DIRECTION('',(0.,1.24327477962315E-16,1.));
#4130=DIRECTION('',(0.,1.24327477962315E-16,1.));
#4131=DIRECTION('',(1.,0.,0.));
#4132=DIRECTION('center_axis',(0.,0.,-1.));
#4133=DIRECTION('ref_axis',(0.,1.,0.));
#4134=DIRECTION('',(0.,1.,0.));
#4135=DIRECTION('',(0.,1.,0.));
#4136=DIRECTION('',(1.,0.,0.));
#4137=DIRECTION('center_axis',(0.,-1.,0.));
#4138=DIRECTION('ref_axis',(0.,0.,-1.));
#4139=DIRECTION('',(0.,0.,-1.));
#4140=DIRECTION('',(0.,0.,-1.));
#4141=DIRECTION('center_axis',(1.,0.,0.));
#4142=DIRECTION('ref_axis',(0.,0.,-1.));
#4143=DIRECTION('center_axis',(1.,0.,0.));
#4144=DIRECTION('ref_axis',(0.,1.,0.));
#4145=DIRECTION('',(1.,-1.22464679914735E-16,0.));
#4146=DIRECTION('',(0.,0.,1.));
#4147=DIRECTION('',(1.,-1.22464679914735E-16,0.));
#4148=DIRECTION('',(0.,0.,1.));
#4149=DIRECTION('',(-1.,0.,0.));
#4150=DIRECTION('',(0.,0.,1.));
#4151=DIRECTION('',(-1.,0.,0.));
#4152=DIRECTION('',(0.,0.,1.));
#4153=DIRECTION('',(0.,0.,1.));
#4154=DIRECTION('',(1.,0.,0.));
#4155=DIRECTION('',(0.,0.,1.));
#4156=DIRECTION('',(1.,0.,0.));
#4157=DIRECTION('',(0.,0.,1.));
#4158=DIRECTION('',(1.,0.,0.));
#4159=DIRECTION('',(0.,0.,1.));
#4160=DIRECTION('',(1.,0.,0.));
#4161=DIRECTION('',(0.,0.,1.));
#4162=DIRECTION('',(1.,0.,0.));
#4163=DIRECTION('',(0.,0.,1.));
#4164=DIRECTION('',(1.,0.,0.));
#4165=CARTESIAN_POINT('',(0.,0.,0.));
#4166=CARTESIAN_POINT('',(0.,0.,0.));
#4167=CARTESIAN_POINT('Origin',(0.,0.,-4.87731));
#4168=CARTESIAN_POINT('',(0.966750000000005,1.1839272930757E-16,-4.80385688672847));
#4169=CARTESIAN_POINT('Origin',(5.11071050262126E-15,0.,-4.80385688672847));
#4170=CARTESIAN_POINT('',(0.754619999999998,-9.24142967572573E-17,-5.));
#4171=CARTESIAN_POINT('',(0.887310000000001,1.08664135135144E-16,-4.87731));
#4172=CARTESIAN_POINT('Origin',(0.,0.,-5.));
#4173=CARTESIAN_POINT('Origin',(-1.91497771928438E-15,0.,1.79999999999952));
#4174=CARTESIAN_POINT('',(1.89999999999999,-2.32682891837997E-16,1.79999999999953));
#4175=CARTESIAN_POINT('Origin',(-1.91497771928438E-15,0.,1.79999999999952));
#4176=CARTESIAN_POINT('',(1.69999999999999,-2.0818995585505E-16,1.99999999999953));
#4177=CARTESIAN_POINT('Origin',(1.7,-2.0818995585505E-16,1.79999999999952));
#4178=CARTESIAN_POINT('Origin',(-2.12775302142714E-15,0.,1.99999999999952));
#4179=CARTESIAN_POINT('Origin',(-1.9,0.,1.99999999999952));
#4180=CARTESIAN_POINT('',(0.75,-0.433012701892219,2.));
#4181=CARTESIAN_POINT('',(1.38777878078145E-16,-0.866025403784439,2.));
#4182=CARTESIAN_POINT('',(-0.149999999999999,-0.952627944162883,1.99999999999952));
#4183=CARTESIAN_POINT('',(-0.750000000000001,-0.433012701892219,2.));
#4184=CARTESIAN_POINT('',(-0.899999999999999,-0.346410161513776,1.99999999999952));
#4185=CARTESIAN_POINT('',(-0.75,0.43301270189222,2.));
#4186=CARTESIAN_POINT('',(-0.75,-0.21650635094611,1.99999999999952));
#4187=CARTESIAN_POINT('',(1.73472347597681E-17,0.866025403784439,2.));
#4188=CARTESIAN_POINT('',(-1.275,0.129903810567666,1.99999999999952));
#4189=CARTESIAN_POINT('',(0.75,0.433012701892219,2.));
#4190=CARTESIAN_POINT('',(-0.524999999999999,1.16913429510899,1.99999999999952));
#4191=CARTESIAN_POINT('',(0.75,0.216506350946109,1.99999999999952));
#4192=CARTESIAN_POINT('Origin',(-1.06387651071333E-15,0.,0.999999999999538));
#4193=CARTESIAN_POINT('',(1.9,-2.32682891837997E-16,-4.47419878923938E-13));
#4194=CARTESIAN_POINT('Origin',(4.74691816123085E-28,0.,-4.48558184615945E-13));
#4195=CARTESIAN_POINT('',(1.9,-2.32682891837997E-16,0.99999999999954));
#4196=CARTESIAN_POINT('Origin',(1.38777878078145E-16,-0.866025403784439,
1.));
#4197=CARTESIAN_POINT('',(1.38777878078145E-16,-0.866025403784439,1.));
#4198=CARTESIAN_POINT('',(0.,2.77555756156289E-16,0.934383502355557));
#4199=CARTESIAN_POINT('',(0.,-0.650754856401699,0.983689509218169));
#4200=CARTESIAN_POINT('',(0.75,-0.433012701892219,1.));
#4201=CARTESIAN_POINT('',(8.5846548499269E-17,-0.866025403784439,1.));
#4202=CARTESIAN_POINT('',(0.563570237279966,-0.325377428200849,0.983689509218169));
#4203=CARTESIAN_POINT('Origin',(0.75,-0.433012701892219,1.));
#4204=CARTESIAN_POINT('',(0.75,0.433012701892219,1.));
#4205=CARTESIAN_POINT('',(0.75,-0.433012701892219,1.));
#4206=CARTESIAN_POINT('',(0.563570237279966,0.32537742820085,0.983689509218169));
#4207=CARTESIAN_POINT('Origin',(0.75,0.433012701892219,1.));
#4208=CARTESIAN_POINT('',(0.,0.866025403784439,1.));
#4209=CARTESIAN_POINT('',(0.75,0.433012701892219,1.));
#4210=CARTESIAN_POINT('',(0.,0.650754856401699,0.983689509218169));
#4211=CARTESIAN_POINT('Origin',(0.,0.866025403784439,1.));
#4212=CARTESIAN_POINT('',(-0.75,0.43301270189222,1.));
#4213=CARTESIAN_POINT('',(1.73472347597681E-17,0.866025403784439,1.));
#4214=CARTESIAN_POINT('',(-0.563570237279966,0.325377428200849,0.983689509218169));
#4215=CARTESIAN_POINT('Origin',(-0.75,0.43301270189222,1.));
#4216=CARTESIAN_POINT('',(-0.750000000000001,-0.433012701892219,1.));
#4217=CARTESIAN_POINT('',(-0.75,0.43301270189222,1.));
#4218=CARTESIAN_POINT('',(-0.563570237279966,-0.325377428200849,0.983689509218169));
#4219=CARTESIAN_POINT('Origin',(-0.750000000000001,-0.433012701892219,1.));
#4220=CARTESIAN_POINT('',(-0.750000000000001,-0.433012701892219,1.));
#4221=CARTESIAN_POINT('Origin',(0.75,-0.433012701892219,2.));
#4222=CARTESIAN_POINT('',(0.75,-0.433012701892219,2.));
#4223=CARTESIAN_POINT('',(1.38777878078145E-16,-0.866025403784439,2.));
#4224=CARTESIAN_POINT('Origin',(0.75,0.433012701892219,2.));
#4225=CARTESIAN_POINT('',(0.75,0.433012701892219,2.));
#4226=CARTESIAN_POINT('Origin',(0.,0.866025403784439,2.));
#4227=CARTESIAN_POINT('',(1.73472347597681E-17,0.866025403784439,2.));
#4228=CARTESIAN_POINT('Origin',(-0.75,0.43301270189222,2.));
#4229=CARTESIAN_POINT('',(-0.75,0.43301270189222,2.));
#4230=CARTESIAN_POINT('Origin',(-0.750000000000001,-0.433012701892219,2.));
#4231=CARTESIAN_POINT('',(-0.750000000000001,-0.433012701892219,2.));
#4232=CARTESIAN_POINT('Origin',(1.38777878078145E-16,-0.866025403784439,
2.));
#4233=CARTESIAN_POINT('Origin',(2.65969127678468E-15,0.,-2.50000000000012));
#4234=CARTESIAN_POINT('',(0.96675,1.1839272930757E-16,-2.35150733091162E-13));
#4235=CARTESIAN_POINT('',(0.966750000000003,-1.1839272930757E-16,-2.50000000000012));
#4236=CARTESIAN_POINT('Origin',(2.48491185144619E-28,0.,-2.35922392732846E-13));
#4237=CARTESIAN_POINT('Origin',(5.27355936696949E-15,0.,-5.));
#4238=CARTESIAN_POINT('Origin',(-0.999999999999996,0.,-2.37147131571737E-13));
#4239=CARTESIAN_POINT('',(0.,0.,0.));
#4240=CARTESIAN_POINT('Origin',(0.,0.,-4.87731));
#4241=CARTESIAN_POINT('',(0.966750000000005,1.1839272930757E-16,-4.80385688672847));
#4242=CARTESIAN_POINT('Origin',(5.11071050262126E-15,0.,-4.80385688672847));
#4243=CARTESIAN_POINT('',(0.754619999999998,-9.24142967572573E-17,-5.));
#4244=CARTESIAN_POINT('',(0.887310000000001,1.08664135135144E-16,-4.87731));
#4245=CARTESIAN_POINT('Origin',(0.,0.,-5.));
#4246=CARTESIAN_POINT('Origin',(-1.91497771928438E-15,0.,1.79999999999952));
#4247=CARTESIAN_POINT('',(1.89999999999999,-2.32682891837997E-16,1.79999999999953));
#4248=CARTESIAN_POINT('Origin',(-1.91497771928438E-15,0.,1.79999999999952));
#4249=CARTESIAN_POINT('',(1.69999999999999,-2.0818995585505E-16,1.99999999999953));
#4250=CARTESIAN_POINT('Origin',(1.7,-2.0818995585505E-16,1.79999999999952));
#4251=CARTESIAN_POINT('Origin',(-2.12775302142714E-15,0.,1.99999999999952));
#4252=CARTESIAN_POINT('Origin',(-1.9,0.,1.99999999999952));
#4253=CARTESIAN_POINT('',(0.75,-0.433012701892219,2.));
#4254=CARTESIAN_POINT('',(1.38777878078145E-16,-0.866025403784439,2.));
#4255=CARTESIAN_POINT('',(-0.149999999999999,-0.952627944162883,1.99999999999952));
#4256=CARTESIAN_POINT('',(-0.750000000000001,-0.433012701892219,2.));
#4257=CARTESIAN_POINT('',(-0.899999999999999,-0.346410161513776,1.99999999999952));
#4258=CARTESIAN_POINT('',(-0.75,0.43301270189222,2.));
#4259=CARTESIAN_POINT('',(-0.75,-0.21650635094611,1.99999999999952));
#4260=CARTESIAN_POINT('',(1.73472347597681E-17,0.866025403784439,2.));
#4261=CARTESIAN_POINT('',(-1.275,0.129903810567666,1.99999999999952));
#4262=CARTESIAN_POINT('',(0.75,0.433012701892219,2.));
#4263=CARTESIAN_POINT('',(-0.524999999999999,1.16913429510899,1.99999999999952));
#4264=CARTESIAN_POINT('',(0.75,0.216506350946109,1.99999999999952));
#4265=CARTESIAN_POINT('Origin',(-1.06387651071333E-15,0.,0.999999999999538));
#4266=CARTESIAN_POINT('',(1.9,-2.32682891837997E-16,-4.47419878923938E-13));
#4267=CARTESIAN_POINT('Origin',(4.74691816123085E-28,0.,-4.48558184615945E-13));
#4268=CARTESIAN_POINT('',(1.9,-2.32682891837997E-16,0.99999999999954));
#4269=CARTESIAN_POINT('Origin',(1.38777878078145E-16,-0.866025403784439,
1.));
#4270=CARTESIAN_POINT('',(1.38777878078145E-16,-0.866025403784439,1.));
#4271=CARTESIAN_POINT('',(0.,2.77555756156289E-16,0.934383502355557));
#4272=CARTESIAN_POINT('',(0.,-0.650754856401699,0.983689509218169));
#4273=CARTESIAN_POINT('',(0.75,-0.433012701892219,1.));
#4274=CARTESIAN_POINT('',(8.5846548499269E-17,-0.866025403784439,1.));
#4275=CARTESIAN_POINT('',(0.563570237279966,-0.325377428200849,0.983689509218169));
#4276=CARTESIAN_POINT('Origin',(0.75,-0.433012701892219,1.));
#4277=CARTESIAN_POINT('',(0.75,0.433012701892219,1.));
#4278=CARTESIAN_POINT('',(0.75,-0.433012701892219,1.));
#4279=CARTESIAN_POINT('',(0.563570237279966,0.32537742820085,0.983689509218169));
#4280=CARTESIAN_POINT('Origin',(0.75,0.433012701892219,1.));
#4281=CARTESIAN_POINT('',(0.,0.866025403784439,1.));
#4282=CARTESIAN_POINT('',(0.75,0.433012701892219,1.));
#4283=CARTESIAN_POINT('',(0.,0.650754856401699,0.983689509218169));
#4284=CARTESIAN_POINT('Origin',(0.,0.866025403784439,1.));
#4285=CARTESIAN_POINT('',(-0.75,0.43301270189222,1.));
#4286=CARTESIAN_POINT('',(1.73472347597681E-17,0.866025403784439,1.));
#4287=CARTESIAN_POINT('',(-0.563570237279966,0.325377428200849,0.983689509218169));
#4288=CARTESIAN_POINT('Origin',(-0.75,0.43301270189222,1.));
#4289=CARTESIAN_POINT('',(-0.750000000000001,-0.433012701892219,1.));
#4290=CARTESIAN_POINT('',(-0.75,0.43301270189222,1.));
#4291=CARTESIAN_POINT('',(-0.563570237279966,-0.325377428200849,0.983689509218169));
#4292=CARTESIAN_POINT('Origin',(-0.750000000000001,-0.433012701892219,1.));
#4293=CARTESIAN_POINT('',(-0.750000000000001,-0.433012701892219,1.));
#4294=CARTESIAN_POINT('Origin',(0.75,-0.433012701892219,2.));
#4295=CARTESIAN_POINT('',(0.75,-0.433012701892219,2.));
#4296=CARTESIAN_POINT('',(1.38777878078145E-16,-0.866025403784439,2.));
#4297=CARTESIAN_POINT('Origin',(0.75,0.433012701892219,2.));
#4298=CARTESIAN_POINT('',(0.75,0.433012701892219,2.));
#4299=CARTESIAN_POINT('Origin',(0.,0.866025403784439,2.));
#4300=CARTESIAN_POINT('',(1.73472347597681E-17,0.866025403784439,2.));
#4301=CARTESIAN_POINT('Origin',(-0.75,0.43301270189222,2.));
#4302=CARTESIAN_POINT('',(-0.75,0.43301270189222,2.));
#4303=CARTESIAN_POINT('Origin',(-0.750000000000001,-0.433012701892219,2.));
#4304=CARTESIAN_POINT('',(-0.750000000000001,-0.433012701892219,2.));
#4305=CARTESIAN_POINT('Origin',(1.38777878078145E-16,-0.866025403784439,
2.));
#4306=CARTESIAN_POINT('Origin',(2.65969127678468E-15,0.,-2.50000000000012));
#4307=CARTESIAN_POINT('',(0.96675,1.1839272930757E-16,-2.35150733091162E-13));
#4308=CARTESIAN_POINT('',(0.966750000000003,-1.1839272930757E-16,-2.50000000000012));
#4309=CARTESIAN_POINT('Origin',(2.48491185144619E-28,0.,-2.35922392732846E-13));
#4310=CARTESIAN_POINT('Origin',(5.27355936696949E-15,0.,-5.));
#4311=CARTESIAN_POINT('Origin',(-0.999999999999996,0.,-2.37147131571737E-13));
#4312=CARTESIAN_POINT('',(0.,0.,0.));
#4313=CARTESIAN_POINT('Origin',(0.,0.,-4.87731));
#4314=CARTESIAN_POINT('',(0.966750000000005,1.1839272930757E-16,-4.80385688672847));
#4315=CARTESIAN_POINT('Origin',(5.11071050262126E-15,0.,-4.80385688672847));
#4316=CARTESIAN_POINT('',(0.754619999999998,-9.24142967572573E-17,-5.));
#4317=CARTESIAN_POINT('',(0.887310000000001,1.08664135135144E-16,-4.87731));
#4318=CARTESIAN_POINT('Origin',(0.,0.,-5.));
#4319=CARTESIAN_POINT('Origin',(-1.91497771928438E-15,0.,1.79999999999952));
#4320=CARTESIAN_POINT('',(1.89999999999999,-2.32682891837997E-16,1.79999999999953));
#4321=CARTESIAN_POINT('Origin',(-1.91497771928438E-15,0.,1.79999999999952));
#4322=CARTESIAN_POINT('',(1.69999999999999,-2.0818995585505E-16,1.99999999999953));
#4323=CARTESIAN_POINT('Origin',(1.7,-2.0818995585505E-16,1.79999999999952));
#4324=CARTESIAN_POINT('Origin',(-2.12775302142714E-15,0.,1.99999999999952));
#4325=CARTESIAN_POINT('Origin',(-1.9,0.,1.99999999999952));
#4326=CARTESIAN_POINT('',(0.75,-0.433012701892219,2.));
#4327=CARTESIAN_POINT('',(1.38777878078145E-16,-0.866025403784439,2.));
#4328=CARTESIAN_POINT('',(-0.149999999999999,-0.952627944162883,1.99999999999952));
#4329=CARTESIAN_POINT('',(-0.750000000000001,-0.433012701892219,2.));
#4330=CARTESIAN_POINT('',(-0.899999999999999,-0.346410161513776,1.99999999999952));
#4331=CARTESIAN_POINT('',(-0.75,0.43301270189222,2.));
#4332=CARTESIAN_POINT('',(-0.75,-0.21650635094611,1.99999999999952));
#4333=CARTESIAN_POINT('',(1.73472347597681E-17,0.866025403784439,2.));
#4334=CARTESIAN_POINT('',(-1.275,0.129903810567666,1.99999999999952));
#4335=CARTESIAN_POINT('',(0.75,0.433012701892219,2.));
#4336=CARTESIAN_POINT('',(-0.524999999999999,1.16913429510899,1.99999999999952));
#4337=CARTESIAN_POINT('',(0.75,0.216506350946109,1.99999999999952));
#4338=CARTESIAN_POINT('Origin',(-1.06387651071333E-15,0.,0.999999999999538));
#4339=CARTESIAN_POINT('',(1.9,-2.32682891837997E-16,-4.47419878923938E-13));
#4340=CARTESIAN_POINT('Origin',(4.74691816123085E-28,0.,-4.48558184615945E-13));
#4341=CARTESIAN_POINT('',(1.9,-2.32682891837997E-16,0.99999999999954));
#4342=CARTESIAN_POINT('Origin',(1.38777878078145E-16,-0.866025403784439,
1.));
#4343=CARTESIAN_POINT('',(1.38777878078145E-16,-0.866025403784439,1.));
#4344=CARTESIAN_POINT('',(0.,2.77555756156289E-16,0.934383502355557));
#4345=CARTESIAN_POINT('',(0.,-0.650754856401699,0.983689509218169));
#4346=CARTESIAN_POINT('',(0.75,-0.433012701892219,1.));
#4347=CARTESIAN_POINT('',(8.5846548499269E-17,-0.866025403784439,1.));
#4348=CARTESIAN_POINT('',(0.563570237279966,-0.325377428200849,0.983689509218169));
#4349=CARTESIAN_POINT('Origin',(0.75,-0.433012701892219,1.));
#4350=CARTESIAN_POINT('',(0.75,0.433012701892219,1.));
#4351=CARTESIAN_POINT('',(0.75,-0.433012701892219,1.));
#4352=CARTESIAN_POINT('',(0.563570237279966,0.32537742820085,0.983689509218169));
#4353=CARTESIAN_POINT('Origin',(0.75,0.433012701892219,1.));
#4354=CARTESIAN_POINT('',(0.,0.866025403784439,1.));
#4355=CARTESIAN_POINT('',(0.75,0.433012701892219,1.));
#4356=CARTESIAN_POINT('',(0.,0.650754856401699,0.983689509218169));
#4357=CARTESIAN_POINT('Origin',(0.,0.866025403784439,1.));
#4358=CARTESIAN_POINT('',(-0.75,0.43301270189222,1.));
#4359=CARTESIAN_POINT('',(1.73472347597681E-17,0.866025403784439,1.));
#4360=CARTESIAN_POINT('',(-0.563570237279966,0.325377428200849,0.983689509218169));
#4361=CARTESIAN_POINT('Origin',(-0.75,0.43301270189222,1.));
#4362=CARTESIAN_POINT('',(-0.750000000000001,-0.433012701892219,1.));
#4363=CARTESIAN_POINT('',(-0.75,0.43301270189222,1.));
#4364=CARTESIAN_POINT('',(-0.563570237279966,-0.325377428200849,0.983689509218169));
#4365=CARTESIAN_POINT('Origin',(-0.750000000000001,-0.433012701892219,1.));
#4366=CARTESIAN_POINT('',(-0.750000000000001,-0.433012701892219,1.));
#4367=CARTESIAN_POINT('Origin',(0.75,-0.433012701892219,2.));
#4368=CARTESIAN_POINT('',(0.75,-0.433012701892219,2.));
#4369=CARTESIAN_POINT('',(1.38777878078145E-16,-0.866025403784439,2.));
#4370=CARTESIAN_POINT('Origin',(0.75,0.433012701892219,2.));
#4371=CARTESIAN_POINT('',(0.75,0.433012701892219,2.));
#4372=CARTESIAN_POINT('Origin',(0.,0.866025403784439,2.));
#4373=CARTESIAN_POINT('',(1.73472347597681E-17,0.866025403784439,2.));
#4374=CARTESIAN_POINT('Origin',(-0.75,0.43301270189222,2.));
#4375=CARTESIAN_POINT('',(-0.75,0.43301270189222,2.));
#4376=CARTESIAN_POINT('Origin',(-0.750000000000001,-0.433012701892219,2.));
#4377=CARTESIAN_POINT('',(-0.750000000000001,-0.433012701892219,2.));
#4378=CARTESIAN_POINT('Origin',(1.38777878078145E-16,-0.866025403784439,
2.));
#4379=CARTESIAN_POINT('Origin',(2.65969127678468E-15,0.,-2.50000000000012));
#4380=CARTESIAN_POINT('',(0.96675,1.1839272930757E-16,-2.35150733091162E-13));
#4381=CARTESIAN_POINT('',(0.966750000000003,-1.1839272930757E-16,-2.50000000000012));
#4382=CARTESIAN_POINT('Origin',(2.48491185144619E-28,0.,-2.35922392732846E-13));
#4383=CARTESIAN_POINT('Origin',(5.27355936696949E-15,0.,-5.));
#4384=CARTESIAN_POINT('Origin',(-0.999999999999996,0.,-2.37147131571737E-13));
#4385=CARTESIAN_POINT('',(0.,0.,0.));
#4386=CARTESIAN_POINT('Origin',(0.,0.,-4.87731));
#4387=CARTESIAN_POINT('',(0.966750000000005,1.1839272930757E-16,-4.80385688672847));
#4388=CARTESIAN_POINT('Origin',(5.11071050262126E-15,0.,-4.80385688672847));
#4389=CARTESIAN_POINT('',(0.754619999999998,-9.24142967572573E-17,-5.));
#4390=CARTESIAN_POINT('',(0.887310000000001,1.08664135135144E-16,-4.87731));
#4391=CARTESIAN_POINT('Origin',(0.,0.,-5.));
#4392=CARTESIAN_POINT('Origin',(-1.91497771928438E-15,0.,1.79999999999952));
#4393=CARTESIAN_POINT('',(1.89999999999999,-2.32682891837997E-16,1.79999999999953));
#4394=CARTESIAN_POINT('Origin',(-1.91497771928438E-15,0.,1.79999999999952));
#4395=CARTESIAN_POINT('',(1.69999999999999,-2.0818995585505E-16,1.99999999999953));
#4396=CARTESIAN_POINT('Origin',(1.7,-2.0818995585505E-16,1.79999999999952));
#4397=CARTESIAN_POINT('Origin',(-2.12775302142714E-15,0.,1.99999999999952));
#4398=CARTESIAN_POINT('Origin',(-1.9,0.,1.99999999999952));
#4399=CARTESIAN_POINT('',(0.75,-0.433012701892219,2.));
#4400=CARTESIAN_POINT('',(1.38777878078145E-16,-0.866025403784439,2.));
#4401=CARTESIAN_POINT('',(-0.149999999999999,-0.952627944162883,1.99999999999952));
#4402=CARTESIAN_POINT('',(-0.750000000000001,-0.433012701892219,2.));
#4403=CARTESIAN_POINT('',(-0.899999999999999,-0.346410161513776,1.99999999999952));
#4404=CARTESIAN_POINT('',(-0.75,0.43301270189222,2.));
#4405=CARTESIAN_POINT('',(-0.75,-0.21650635094611,1.99999999999952));
#4406=CARTESIAN_POINT('',(1.73472347597681E-17,0.866025403784439,2.));
#4407=CARTESIAN_POINT('',(-1.275,0.129903810567666,1.99999999999952));
#4408=CARTESIAN_POINT('',(0.75,0.433012701892219,2.));
#4409=CARTESIAN_POINT('',(-0.524999999999999,1.16913429510899,1.99999999999952));
#4410=CARTESIAN_POINT('',(0.75,0.216506350946109,1.99999999999952));
#4411=CARTESIAN_POINT('Origin',(-1.06387651071333E-15,0.,0.999999999999538));
#4412=CARTESIAN_POINT('',(1.9,-2.32682891837997E-16,-4.47419878923938E-13));
#4413=CARTESIAN_POINT('Origin',(4.74691816123085E-28,0.,-4.48558184615945E-13));
#4414=CARTESIAN_POINT('',(1.9,-2.32682891837997E-16,0.99999999999954));
#4415=CARTESIAN_POINT('Origin',(1.38777878078145E-16,-0.866025403784439,
1.));
#4416=CARTESIAN_POINT('',(1.38777878078145E-16,-0.866025403784439,1.));
#4417=CARTESIAN_POINT('',(0.,2.77555756156289E-16,0.934383502355557));
#4418=CARTESIAN_POINT('',(0.,-0.650754856401699,0.983689509218169));
#4419=CARTESIAN_POINT('',(0.75,-0.433012701892219,1.));
#4420=CARTESIAN_POINT('',(8.5846548499269E-17,-0.866025403784439,1.));
#4421=CARTESIAN_POINT('',(0.563570237279966,-0.325377428200849,0.983689509218169));
#4422=CARTESIAN_POINT('Origin',(0.75,-0.433012701892219,1.));
#4423=CARTESIAN_POINT('',(0.75,0.433012701892219,1.));
#4424=CARTESIAN_POINT('',(0.75,-0.433012701892219,1.));
#4425=CARTESIAN_POINT('',(0.563570237279966,0.32537742820085,0.983689509218169));
#4426=CARTESIAN_POINT('Origin',(0.75,0.433012701892219,1.));
#4427=CARTESIAN_POINT('',(0.,0.866025403784439,1.));
#4428=CARTESIAN_POINT('',(0.75,0.433012701892219,1.));
#4429=CARTESIAN_POINT('',(0.,0.650754856401699,0.983689509218169));
#4430=CARTESIAN_POINT('Origin',(0.,0.866025403784439,1.));
#4431=CARTESIAN_POINT('',(-0.75,0.43301270189222,1.));
#4432=CARTESIAN_POINT('',(1.73472347597681E-17,0.866025403784439,1.));
#4433=CARTESIAN_POINT('',(-0.563570237279966,0.325377428200849,0.983689509218169));
#4434=CARTESIAN_POINT('Origin',(-0.75,0.43301270189222,1.));
#4435=CARTESIAN_POINT('',(-0.750000000000001,-0.433012701892219,1.));
#4436=CARTESIAN_POINT('',(-0.75,0.43301270189222,1.));
#4437=CARTESIAN_POINT('',(-0.563570237279966,-0.325377428200849,0.983689509218169));
#4438=CARTESIAN_POINT('Origin',(-0.750000000000001,-0.433012701892219,1.));
#4439=CARTESIAN_POINT('',(-0.750000000000001,-0.433012701892219,1.));
#4440=CARTESIAN_POINT('Origin',(0.75,-0.433012701892219,2.));
#4441=CARTESIAN_POINT('',(0.75,-0.433012701892219,2.));
#4442=CARTESIAN_POINT('',(1.38777878078145E-16,-0.866025403784439,2.));
#4443=CARTESIAN_POINT('Origin',(0.75,0.433012701892219,2.));
#4444=CARTESIAN_POINT('',(0.75,0.433012701892219,2.));
#4445=CARTESIAN_POINT('Origin',(0.,0.866025403784439,2.));
#4446=CARTESIAN_POINT('',(1.73472347597681E-17,0.866025403784439,2.));
#4447=CARTESIAN_POINT('Origin',(-0.75,0.43301270189222,2.));
#4448=CARTESIAN_POINT('',(-0.75,0.43301270189222,2.));
#4449=CARTESIAN_POINT('Origin',(-0.750000000000001,-0.433012701892219,2.));
#4450=CARTESIAN_POINT('',(-0.750000000000001,-0.433012701892219,2.));
#4451=CARTESIAN_POINT('Origin',(1.38777878078145E-16,-0.866025403784439,
2.));
#4452=CARTESIAN_POINT('Origin',(2.65969127678468E-15,0.,-2.50000000000012));
#4453=CARTESIAN_POINT('',(0.96675,1.1839272930757E-16,-2.35150733091162E-13));
#4454=CARTESIAN_POINT('',(0.966750000000003,-1.1839272930757E-16,-2.50000000000012));
#4455=CARTESIAN_POINT('Origin',(2.48491185144619E-28,0.,-2.35922392732846E-13));
#4456=CARTESIAN_POINT('Origin',(5.27355936696949E-15,0.,-5.));
#4457=CARTESIAN_POINT('Origin',(-0.999999999999996,0.,-2.37147131571737E-13));
#4458=CARTESIAN_POINT('',(0.,0.,0.));
#4459=CARTESIAN_POINT('Origin',(-40.,0.,-3.02305319600895));
#4460=CARTESIAN_POINT('',(-38.5,1.83697019872103E-16,-2.77305319600895));
#4461=CARTESIAN_POINT('Origin',(-40.,0.,-2.77305319600895));
#4462=CARTESIAN_POINT('',(-38.,-2.44929359829471E-16,-3.27305319600895));
#4463=CARTESIAN_POINT('',(-38.25,-2.14313189850787E-16,-3.02305319600895));
#4464=CARTESIAN_POINT('Origin',(-40.,0.,-3.27305319600895));
#4465=CARTESIAN_POINT('Origin',(0.,0.,-3.27305319600895));
#4466=CARTESIAN_POINT('',(-50.,4.52151022278658,-3.27305319600895));
#4467=CARTESIAN_POINT('',(50.,4.52151022278658,-3.27305319600895));
#4468=CARTESIAN_POINT('',(0.,4.52151022278658,-3.27305319600895));
#4469=CARTESIAN_POINT('',(50.,-4.52151022278658,-3.27305319600895));
#4470=CARTESIAN_POINT('',(50.,-4.52151022278658,-3.27305319600895));
#4471=CARTESIAN_POINT('',(-50.,-4.52151022278658,-3.27305319600895));
#4472=CARTESIAN_POINT('',(0.,-4.52151022278658,-3.27305319600895));
#4473=CARTESIAN_POINT('',(-50.,4.52151022278658,-3.27305319600895));
#4474=CARTESIAN_POINT('',(-18.,-2.4492935982947E-16,-3.27305319600895));
#4475=CARTESIAN_POINT('Origin',(-20.,0.,-3.27305319600895));
#4476=CARTESIAN_POINT('',(22.,-2.44929359829471E-16,-3.27305319600895));
#4477=CARTESIAN_POINT('Origin',(20.,0.,-3.27305319600895));
#4478=CARTESIAN_POINT('',(42.,-2.4492935982947E-16,-3.27305319600895));
#4479=CARTESIAN_POINT('Origin',(40.,0.,-3.27305319600895));
#4480=CARTESIAN_POINT('',(2.,-2.44929359829471E-16,-3.27305319600895));
#4481=CARTESIAN_POINT('Origin',(0.,0.,-3.27305319600895));
#4482=CARTESIAN_POINT('Origin',(-40.,0.,3.27472668609763));
#4483=CARTESIAN_POINT('',(-38.5,1.83697019872103E-16,1.27472668609763));
#4484=CARTESIAN_POINT('Origin',(-40.,0.,1.27472668609763));
#4485=CARTESIAN_POINT('',(-38.5,-1.83697019872103E-16,3.27472668609763));
#4486=CARTESIAN_POINT('Origin',(-20.,0.,-3.02305319600895));
#4487=CARTESIAN_POINT('',(-18.5,1.83697019872103E-16,-2.77305319600895));
#4488=CARTESIAN_POINT('Origin',(-20.,0.,-2.77305319600895));
#4489=CARTESIAN_POINT('',(-18.25,-2.14313189850787E-16,-3.02305319600895));
#4490=CARTESIAN_POINT('Origin',(-20.,0.,3.27472668609763));
#4491=CARTESIAN_POINT('',(-18.5,1.83697019872103E-16,1.27472668609763));
#4492=CARTESIAN_POINT('Origin',(-20.,0.,1.27472668609763));
#4493=CARTESIAN_POINT('',(-18.5,-1.83697019872103E-16,3.27472668609763));
#4494=CARTESIAN_POINT('Origin',(0.,0.,-3.02305319600895));
#4495=CARTESIAN_POINT('',(1.5,1.83697019872103E-16,-2.77305319600895));
#4496=CARTESIAN_POINT('Origin',(0.,0.,-2.77305319600895));
#4497=CARTESIAN_POINT('',(1.75,-2.14313189850787E-16,-3.02305319600895));
#4498=CARTESIAN_POINT('Origin',(0.,0.,3.27472668609763));
#4499=CARTESIAN_POINT('',(1.5,1.83697019872103E-16,1.27472668609763));
#4500=CARTESIAN_POINT('Origin',(0.,0.,1.27472668609763));
#4501=CARTESIAN_POINT('',(1.5,-1.83697019872103E-16,3.27472668609763));
#4502=CARTESIAN_POINT('Origin',(20.,0.,-3.02305319600895));
#4503=CARTESIAN_POINT('',(21.5,1.83697019872103E-16,-2.77305319600895));
#4504=CARTESIAN_POINT('Origin',(20.,0.,-2.77305319600895));
#4505=CARTESIAN_POINT('',(21.75,-2.14313189850787E-16,-3.02305319600895));
#4506=CARTESIAN_POINT('Origin',(20.,0.,3.27472668609763));
#4507=CARTESIAN_POINT('',(21.5,1.83697019872103E-16,1.27472668609763));
#4508=CARTESIAN_POINT('Origin',(20.,0.,1.27472668609763));
#4509=CARTESIAN_POINT('',(21.5,-1.83697019872103E-16,3.27472668609763));
#4510=CARTESIAN_POINT('Origin',(40.,0.,-3.02305319600895));
#4511=CARTESIAN_POINT('',(41.5,1.83697019872103E-16,-2.77305319600895));
#4512=CARTESIAN_POINT('Origin',(40.,0.,-2.77305319600895));
#4513=CARTESIAN_POINT('',(41.75,-2.14313189850787E-16,-3.02305319600895));
#4514=CARTESIAN_POINT('Origin',(40.,0.,3.27472668609763));
#4515=CARTESIAN_POINT('',(41.5,1.83697019872103E-16,1.27472668609763));
#4516=CARTESIAN_POINT('Origin',(40.,0.,1.27472668609763));
#4517=CARTESIAN_POINT('',(41.5,-1.83697019872103E-16,3.27472668609763));
#4518=CARTESIAN_POINT('Origin',(0.,0.,3.27472668609763));
#4519=CARTESIAN_POINT('',(3.,3.67394039744206E-16,3.27472668609763));
#4520=CARTESIAN_POINT('Origin',(0.,0.,3.27472668609763));
#4521=CARTESIAN_POINT('',(3.,3.67394039744206E-16,1.27472668609763));
#4522=CARTESIAN_POINT('',(3.,-3.67394039744206E-16,3.27472668609763));
#4523=CARTESIAN_POINT('Origin',(0.,0.,1.27472668609763));
#4524=CARTESIAN_POINT('Origin',(0.,0.,1.27472668609763));
#4525=CARTESIAN_POINT('Origin',(20.,0.,3.27472668609763));
#4526=CARTESIAN_POINT('',(23.,3.67394039744206E-16,3.27472668609763));
#4527=CARTESIAN_POINT('Origin',(20.,0.,3.27472668609763));
#4528=CARTESIAN_POINT('',(23.,3.67394039744206E-16,1.27472668609763));
#4529=CARTESIAN_POINT('',(23.,-3.67394039744206E-16,3.27472668609763));
#4530=CARTESIAN_POINT('Origin',(20.,0.,1.27472668609763));
#4531=CARTESIAN_POINT('Origin',(20.,0.,1.27472668609763));
#4532=CARTESIAN_POINT('Origin',(-20.,0.,3.27472668609763));
#4533=CARTESIAN_POINT('',(-17.,3.67394039744206E-16,3.27472668609763));
#4534=CARTESIAN_POINT('Origin',(-20.,0.,3.27472668609763));
#4535=CARTESIAN_POINT('',(-17.,3.67394039744206E-16,1.27472668609763));
#4536=CARTESIAN_POINT('',(-17.,-3.67394039744206E-16,3.27472668609763));
#4537=CARTESIAN_POINT('Origin',(-20.,0.,1.27472668609763));
#4538=CARTESIAN_POINT('Origin',(-20.,0.,1.27472668609763));
#4539=CARTESIAN_POINT('Origin',(40.,0.,3.27472668609763));
#4540=CARTESIAN_POINT('',(43.,3.67394039744206E-16,3.27472668609763));
#4541=CARTESIAN_POINT('Origin',(40.,0.,3.27472668609763));
#4542=CARTESIAN_POINT('',(43.,3.67394039744206E-16,1.27472668609763));
#4543=CARTESIAN_POINT('',(43.,-3.67394039744206E-16,3.27472668609763));
#4544=CARTESIAN_POINT('Origin',(40.,0.,1.27472668609763));
#4545=CARTESIAN_POINT('Origin',(40.,0.,1.27472668609763));
#4546=CARTESIAN_POINT('Origin',(-40.,0.,3.27472668609763));
#4547=CARTESIAN_POINT('',(-37.,3.67394039744206E-16,3.27472668609763));
#4548=CARTESIAN_POINT('Origin',(-40.,0.,3.27472668609763));
#4549=CARTESIAN_POINT('',(-37.,3.67394039744206E-16,1.27472668609763));
#4550=CARTESIAN_POINT('',(-37.,-3.67394039744206E-16,3.27472668609763));
#4551=CARTESIAN_POINT('Origin',(-40.,0.,1.27472668609763));
#4552=CARTESIAN_POINT('Origin',(-40.,0.,1.27472668609763));
#4553=CARTESIAN_POINT('Origin',(0.,-4.52151022278658,1.494186706068));
#4554=CARTESIAN_POINT('',(50.,-4.52151022278658,2.73932600723025));
#4555=CARTESIAN_POINT('',(-50.,-4.52151022278658,2.73932600723025));
#4556=CARTESIAN_POINT('',(0.,-4.52151022278658,2.73932600723025));
#4557=CARTESIAN_POINT('',(-50.,-4.52151022278658,1.494186706068));
#4558=CARTESIAN_POINT('',(-50.,-4.52151022278658,3.27472668609763));
#4559=CARTESIAN_POINT('',(50.,-4.52151022278658,1.494186706068));
#4560=CARTESIAN_POINT('',(0.,-4.52151022278658,1.494186706068));
#4561=CARTESIAN_POINT('',(50.,-4.52151022278658,3.27472668609763));
#4562=CARTESIAN_POINT('Origin',(0.,-4.49107020104243,0.747511725556171));
#4563=CARTESIAN_POINT('',(-50.,-4.52151022278657,0.000836745044343612));
#4564=CARTESIAN_POINT('Origin',(-50.,-4.49107020104243,0.747511725556171));
#4565=CARTESIAN_POINT('',(50.,-4.52151022278657,0.000836745044343612));
#4566=CARTESIAN_POINT('',(0.,-4.52151022278657,0.000836745044343579));
#4567=CARTESIAN_POINT('Origin',(50.,-4.49107020104243,0.747511725556171));
#4568=CARTESIAN_POINT('Origin',(0.,-4.52151022278658,-3.27305319600895));
#4569=CARTESIAN_POINT('',(-50.,-4.52151022278658,3.27472668609763));
#4570=CARTESIAN_POINT('',(50.,-4.52151022278658,3.27472668609763));
#4571=CARTESIAN_POINT('Origin',(0.,-4.52151022278658,2.73932600723025));
#4572=CARTESIAN_POINT('',(-50.,-3.98588327568422,3.27472668609763));
#4573=CARTESIAN_POINT('',(50.,-3.98588327568422,3.27472668609763));
#4574=CARTESIAN_POINT('',(0.,-3.98588327568422,3.27472668609763));
#4575=CARTESIAN_POINT('',(-50.,-4.52151022278658,2.73932600723025));
#4576=CARTESIAN_POINT('',(50.,-4.52151022278658,2.73932600723025));
#4577=CARTESIAN_POINT('Origin',(-50.,2.26075511139329,0.000836745044343612));
#4578=CARTESIAN_POINT('',(-50.,3.98588327568422,3.27472668609763));
#4579=CARTESIAN_POINT('',(-50.,4.52151022278658,2.73932600723025));
#4580=CARTESIAN_POINT('',(-50.,4.52151022278658,2.73932600723025));
#4581=CARTESIAN_POINT('',(-50.,4.52151022278658,1.494186706068));
#4582=CARTESIAN_POINT('',(-50.,4.52151022278658,3.27472668609763));
#4583=CARTESIAN_POINT('',(-50.,4.52151022278657,0.000836745044343612));
#4584=CARTESIAN_POINT('Origin',(-50.,4.49107020104243,0.747511725556171));
#4585=CARTESIAN_POINT('',(-50.,4.52151022278658,3.27472668609763));
#4586=CARTESIAN_POINT('',(-50.,0.,3.27472668609763));
#4587=CARTESIAN_POINT('Origin',(0.,4.52151022278658,1.494186706068));
#4588=CARTESIAN_POINT('',(50.,4.52151022278658,2.73932600723025));
#4589=CARTESIAN_POINT('',(0.,4.52151022278658,2.73932600723025));
#4590=CARTESIAN_POINT('',(50.,4.52151022278658,1.494186706068));
#4591=CARTESIAN_POINT('',(50.,4.52151022278658,3.27472668609763));
#4592=CARTESIAN_POINT('',(0.,4.52151022278658,1.494186706068));
#4593=CARTESIAN_POINT('Origin',(0.,4.49107020104243,0.747511725556171));
#4594=CARTESIAN_POINT('',(50.,4.52151022278657,0.000836745044343612));
#4595=CARTESIAN_POINT('Origin',(50.,4.49107020104243,0.747511725556171));
#4596=CARTESIAN_POINT('',(0.,4.52151022278657,0.000836745044343579));
#4597=CARTESIAN_POINT('Origin',(0.,4.52151022278658,-3.27305319600895));
#4598=CARTESIAN_POINT('',(50.,4.52151022278658,3.27472668609763));
#4599=CARTESIAN_POINT('Origin',(0.,3.98588327568422,3.27472668609763));
#4600=CARTESIAN_POINT('',(50.,3.98588327568422,3.27472668609763));
#4601=CARTESIAN_POINT('',(50.,0.,3.27472668609763));
#4602=CARTESIAN_POINT('',(0.,3.98588327568422,3.27472668609763));
#4603=CARTESIAN_POINT('Origin',(0.,4.52151022278658,2.73932600723025));
#4604=CARTESIAN_POINT('',(50.,4.52151022278658,2.73932600723025));
#4605=CARTESIAN_POINT('Origin',(50.,2.26075511139329,0.000836745044343612));
#4606=CARTESIAN_POINT('',(0.,0.,0.));
#4607=CARTESIAN_POINT('Origin',(4.99661841059868,-7.50651000176462,6.74711402388884));
#4608=CARTESIAN_POINT('',(6.24661841059868,-7.50651000176462,6.74711402388884));
#4609=CARTESIAN_POINT('Origin',(4.99661841059868,-7.50651000176462,6.74711402388884));
#4610=CARTESIAN_POINT('',(6.24661841059868,-7.50651000176462,1.74711402388884));
#4611=CARTESIAN_POINT('',(6.24661841059868,-7.50651000176462,6.74711402388884));
#4612=CARTESIAN_POINT('Origin',(4.99661841059868,-7.50651000176462,1.74711402388884));
#4613=CARTESIAN_POINT('Origin',(4.99661841059868,-7.50651000176462,1.74711402388884));
#4614=CARTESIAN_POINT('Origin',(-4.99661841059868,7.50651000176462,6.74711402388884));
#4615=CARTESIAN_POINT('',(-3.74661841059868,7.50651000176462,6.74711402388884));
#4616=CARTESIAN_POINT('Origin',(-4.99661841059868,7.50651000176462,6.74711402388884));
#4617=CARTESIAN_POINT('',(-3.74661841059868,7.50651000176462,1.74711402388884));
#4618=CARTESIAN_POINT('',(-3.74661841059868,7.50651000176462,6.74711402388884));
#4619=CARTESIAN_POINT('Origin',(-4.99661841059868,7.50651000176462,1.74711402388884));
#4620=CARTESIAN_POINT('Origin',(-4.99661841059868,7.50651000176462,1.74711402388884));
#4621=CARTESIAN_POINT('Origin',(-4.99661841059868,-7.50651000176462,6.74711402388884));
#4622=CARTESIAN_POINT('',(-3.74661841059868,-7.50651000176462,6.74711402388884));
#4623=CARTESIAN_POINT('Origin',(-4.99661841059868,-7.50651000176462,6.74711402388884));
#4624=CARTESIAN_POINT('',(-3.74661841059868,-7.50651000176462,1.74711402388884));
#4625=CARTESIAN_POINT('',(-3.74661841059868,-7.50651000176462,6.74711402388884));
#4626=CARTESIAN_POINT('Origin',(-4.99661841059868,-7.50651000176462,1.74711402388884));
#4627=CARTESIAN_POINT('Origin',(-4.99661841059868,-7.50651000176462,1.74711402388884));
#4628=CARTESIAN_POINT('Origin',(4.99661841059868,7.50651000176462,6.74711402388884));
#4629=CARTESIAN_POINT('',(6.24661841059868,7.50651000176462,6.74711402388884));
#4630=CARTESIAN_POINT('Origin',(4.99661841059868,7.50651000176462,6.74711402388884));
#4631=CARTESIAN_POINT('',(6.24661841059868,7.50651000176462,1.74711402388884));
#4632=CARTESIAN_POINT('',(6.24661841059868,7.50651000176462,6.74711402388884));
#4633=CARTESIAN_POINT('Origin',(4.99661841059868,7.50651000176462,1.74711402388884));
#4634=CARTESIAN_POINT('Origin',(4.99661841059868,7.50651000176462,1.74711402388884));
#4635=CARTESIAN_POINT('Origin',(-9.5,0.,2.75621475582567));
#4636=CARTESIAN_POINT('',(-9.5,4.48396394323217,3.23022961141938));
#4637=CARTESIAN_POINT('',(-9.5,-4.48396394323217,3.23022961141938));
#4638=CARTESIAN_POINT('',(-9.5,0.,3.23022961141938));
#4639=CARTESIAN_POINT('',(-9.5,-4.48396394323217,-1.2346845122375));
#4640=CARTESIAN_POINT('',(-9.5,-4.48396394323217,3.23022961141938));
#4641=CARTESIAN_POINT('',(-9.5,-10.0039433906299,-1.2346845122375));
#4642=CARTESIAN_POINT('',(-9.5,-4.48396394323217,-1.2346845122375));
#4643=CARTESIAN_POINT('',(-9.5,-10.0039433906299,6.74711402388884));
#4644=CARTESIAN_POINT('',(-9.5,-10.0039433906299,-1.2346845122375));
#4645=CARTESIAN_POINT('',(-9.5,-5.01914200599926,6.74711402388884));
#4646=CARTESIAN_POINT('',(-9.5,-10.0039433906299,6.74711402388884));
#4647=CARTESIAN_POINT('',(-9.5,-4.51226721735165,6.26348125396712));
#4648=CARTESIAN_POINT('',(-9.5,-5.01914200599926,6.74711402388884));
#4649=CARTESIAN_POINT('',(-9.5,4.51226721735165,6.26348125396712));
#4650=CARTESIAN_POINT('',(-9.5,4.51226721735165,6.26348125396712));
#4651=CARTESIAN_POINT('',(-9.5,5.01914200599926,6.74711402388884));
#4652=CARTESIAN_POINT('',(-9.5,5.01914200599926,6.74711402388884));
#4653=CARTESIAN_POINT('',(-9.5,10.0039433906299,6.74711402388884));
#4654=CARTESIAN_POINT('',(-9.5,10.0039433906299,6.74711402388884));
#4655=CARTESIAN_POINT('',(-9.5,10.0039433906299,-1.2346845122375));
#4656=CARTESIAN_POINT('',(-9.5,10.0039433906299,-1.2346845122375));
#4657=CARTESIAN_POINT('',(-9.5,4.48396394323217,-1.2346845122375));
#4658=CARTESIAN_POINT('',(-9.5,4.48396394323217,-1.2346845122375));
#4659=CARTESIAN_POINT('',(-9.5,4.48396394323217,3.23022961141938));
#4660=CARTESIAN_POINT('Origin',(0.,-4.48396394323217,-1.2346845122375));
#4661=CARTESIAN_POINT('',(9.5,-4.48396394323217,3.23022961141938));
#4662=CARTESIAN_POINT('',(0.,-4.48396394323217,3.23022961141938));
#4663=CARTESIAN_POINT('',(9.5,-4.48396394323217,-1.2346845122375));
#4664=CARTESIAN_POINT('',(9.5,-4.48396394323217,3.23022961141938));
#4665=CARTESIAN_POINT('',(0.,-4.48396394323217,-1.2346845122375));
#4666=CARTESIAN_POINT('Origin',(0.,-10.0039433906299,-1.2346845122375));
#4667=CARTESIAN_POINT('',(9.5,-10.0039433906299,-1.2346845122375));
#4668=CARTESIAN_POINT('',(9.5,-4.48396394323217,-1.2346845122375));
#4669=CARTESIAN_POINT('',(0.,-10.0039433906299,-1.2346845122375));
#4670=CARTESIAN_POINT('Origin',(0.,-10.0039433906299,6.74711402388884));
#4671=CARTESIAN_POINT('',(9.5,-10.0039433906299,6.74711402388884));
#4672=CARTESIAN_POINT('',(9.5,-10.0039433906299,-1.2346845122375));
#4673=CARTESIAN_POINT('',(0.,-10.0039433906299,6.74711402388884));
#4674=CARTESIAN_POINT('Origin',(0.,-5.01914200599926,6.74711402388884));
#4675=CARTESIAN_POINT('',(9.5,-5.01914200599926,6.74711402388884));
#4676=CARTESIAN_POINT('',(9.5,-10.0039433906299,6.74711402388884));
#4677=CARTESIAN_POINT('',(0.,-5.01914200599926,6.74711402388884));
#4678=CARTESIAN_POINT('Origin',(0.,-4.51226721735165,6.26348125396712));
#4679=CARTESIAN_POINT('',(9.5,-4.51226721735165,6.26348125396712));
#4680=CARTESIAN_POINT('',(9.5,-5.01914200599926,6.74711402388884));
#4681=CARTESIAN_POINT('',(0.,-4.51226721735165,6.26348125396712));
#4682=CARTESIAN_POINT('Origin',(0.,4.51226721735165,6.26348125396712));
#4683=CARTESIAN_POINT('',(9.5,4.51226721735165,6.26348125396712));
#4684=CARTESIAN_POINT('',(9.5,4.51226721735165,6.26348125396712));
#4685=CARTESIAN_POINT('',(0.,4.51226721735165,6.26348125396712));
#4686=CARTESIAN_POINT('Origin',(0.,5.01914200599926,6.74711402388884));
#4687=CARTESIAN_POINT('',(9.5,5.01914200599926,6.74711402388884));
#4688=CARTESIAN_POINT('',(9.5,5.01914200599926,6.74711402388884));
#4689=CARTESIAN_POINT('',(0.,5.01914200599926,6.74711402388884));
#4690=CARTESIAN_POINT('Origin',(0.,10.0039433906299,6.74711402388884));
#4691=CARTESIAN_POINT('',(9.5,10.0039433906299,6.74711402388884));
#4692=CARTESIAN_POINT('',(9.5,10.0039433906299,6.74711402388884));
#4693=CARTESIAN_POINT('',(0.,10.0039433906299,6.74711402388884));
#4694=CARTESIAN_POINT('Origin',(0.,10.0039433906299,-1.2346845122375));
#4695=CARTESIAN_POINT('',(9.5,10.0039433906299,-1.2346845122375));
#4696=CARTESIAN_POINT('',(9.5,10.0039433906299,-1.2346845122375));
#4697=CARTESIAN_POINT('',(0.,10.0039433906299,-1.2346845122375));
#4698=CARTESIAN_POINT('Origin',(0.,4.48396394323217,-1.2346845122375));
#4699=CARTESIAN_POINT('',(9.5,4.48396394323217,-1.2346845122375));
#4700=CARTESIAN_POINT('',(9.5,4.48396394323217,-1.2346845122375));
#4701=CARTESIAN_POINT('',(0.,4.48396394323217,-1.2346845122375));
#4702=CARTESIAN_POINT('Origin',(0.,4.48396394323217,3.23022961141938));
#4703=CARTESIAN_POINT('',(9.5,4.48396394323217,3.23022961141938));
#4704=CARTESIAN_POINT('',(9.5,4.48396394323217,3.23022961141938));
#4705=CARTESIAN_POINT('',(0.,4.48396394323217,3.23022961141938));
#4706=CARTESIAN_POINT('Origin',(0.,-4.48396394323217,3.23022961141938));
#4707=CARTESIAN_POINT('',(9.5,0.,3.23022961141938));
#4708=CARTESIAN_POINT('Origin',(9.5,0.,2.75621475582567));
#4709=CARTESIAN_POINT('',(0.,0.,0.));
#4710=CARTESIAN_POINT('Origin',(-14.5,7.24395366693103,1.75498192028357));
#4711=CARTESIAN_POINT('',(-9.5,6.24395366693103,1.75498192028357));
#4712=CARTESIAN_POINT('Origin',(-9.5,7.24395366693103,1.75498192028357));
#4713=CARTESIAN_POINT('',(-13.5,6.24395366693103,1.75498192028357));
#4714=CARTESIAN_POINT('',(-14.5,6.24395366693103,1.75498192028357));
#4715=CARTESIAN_POINT('Origin',(-13.5,7.24395366693103,1.75498192028357));
#4716=CARTESIAN_POINT('Origin',(-14.5,-7.24395366693103,1.75498192028357));
#4717=CARTESIAN_POINT('',(-9.5,-8.24395366693103,1.75498192028357));
#4718=CARTESIAN_POINT('Origin',(-9.5,-7.24395366693103,1.75498192028357));
#4719=CARTESIAN_POINT('',(-13.5,-8.24395366693103,1.75498192028357));
#4720=CARTESIAN_POINT('',(-14.5,-8.24395366693103,1.75498192028357));
#4721=CARTESIAN_POINT('Origin',(-13.5,-7.24395366693103,1.75498192028357));
#4722=CARTESIAN_POINT('Origin',(-9.5,10.0039433906299,6.26348125396711));
#4723=CARTESIAN_POINT('',(-9.5,10.0039433906299,6.26348125396711));
#4724=CARTESIAN_POINT('',(-9.5,-10.0039433906299,6.26348125396711));
#4725=CARTESIAN_POINT('',(-9.5,10.0039433906299,6.26348125396711));
#4726=CARTESIAN_POINT('',(-13.5,10.0039433906299,6.26348125396711));
#4727=CARTESIAN_POINT('',(-9.5,10.0039433906299,6.26348125396711));
#4728=CARTESIAN_POINT('',(-13.5,-10.0039433906299,6.26348125396711));
#4729=CARTESIAN_POINT('',(-13.5,10.0039433906299,6.26348125396711));
#4730=CARTESIAN_POINT('',(-9.5,-10.0039433906299,6.26348125396711));
#4731=CARTESIAN_POINT('Origin',(-9.5,10.0039433906299,-1.2346845122375));
#4732=CARTESIAN_POINT('',(-9.5,10.0039433906299,-1.2346845122375));
#4733=CARTESIAN_POINT('',(-9.5,10.0039433906299,-1.2346845122375));
#4734=CARTESIAN_POINT('',(-13.5,10.0039433906299,-1.2346845122375));
#4735=CARTESIAN_POINT('',(-9.5,10.0039433906299,-1.2346845122375));
#4736=CARTESIAN_POINT('',(-13.5,10.0039433906299,-1.2346845122375));
#4737=CARTESIAN_POINT('Origin',(-9.5,4.48396394323217,-1.2346845122375));
#4738=CARTESIAN_POINT('',(-9.5,4.48396394323217,-1.2346845122375));
#4739=CARTESIAN_POINT('',(-9.5,-10.0039433906299,-1.2346845122375));
#4740=CARTESIAN_POINT('',(-13.5,4.48396394323217,-1.2346845122375));
#4741=CARTESIAN_POINT('',(-9.5,4.48396394323217,-1.2346845122375));
#4742=CARTESIAN_POINT('',(-13.5,-10.0039433906299,-1.2346845122375));
#4743=CARTESIAN_POINT('Origin',(-9.5,4.48396394323217,3.23022961141938));
#4744=CARTESIAN_POINT('',(-9.5,4.48396394323217,3.23022961141938));
#4745=CARTESIAN_POINT('',(-9.5,4.48396394323217,3.23022961141938));
#4746=CARTESIAN_POINT('',(-13.5,4.48396394323217,3.23022961141938));
#4747=CARTESIAN_POINT('',(-9.5,4.48396394323217,3.23022961141938));
#4748=CARTESIAN_POINT('',(-13.5,4.48396394323217,3.23022961141938));
#4749=CARTESIAN_POINT('Origin',(-9.5,-4.48396394323217,3.23022961141938));
#4750=CARTESIAN_POINT('',(-9.5,-4.48396394323217,3.23022961141938));
#4751=CARTESIAN_POINT('',(-9.5,-4.48396394323217,3.23022961141938));
#4752=CARTESIAN_POINT('',(-13.5,-4.48396394323217,3.23022961141938));
#4753=CARTESIAN_POINT('',(-9.5,-4.48396394323217,3.23022961141938));
#4754=CARTESIAN_POINT('',(-13.5,-4.48396394323217,3.23022961141938));
#4755=CARTESIAN_POINT('Origin',(-9.5,-4.48396394323217,-1.2346845122375));
#4756=CARTESIAN_POINT('',(-9.5,-4.48396394323217,-1.2346845122375));
#4757=CARTESIAN_POINT('',(-9.5,-4.48396394323217,-1.2346845122375));
#4758=CARTESIAN_POINT('',(-13.5,-4.48396394323217,-1.2346845122375));
#4759=CARTESIAN_POINT('',(-9.5,-4.48396394323217,-1.2346845122375));
#4760=CARTESIAN_POINT('',(-13.5,-4.48396394323217,-1.2346845122375));
#4761=CARTESIAN_POINT('Origin',(-9.5,-10.0039433906299,-1.2346845122375));
#4762=CARTESIAN_POINT('',(-9.5,-10.0039433906299,-1.2346845122375));
#4763=CARTESIAN_POINT('',(-9.5,-10.0039433906299,-1.2346845122375));
#4764=CARTESIAN_POINT('',(-13.5,-10.0039433906299,-1.2346845122375));
#4765=CARTESIAN_POINT('',(-9.5,-10.0039433906299,-1.2346845122375));
#4766=CARTESIAN_POINT('',(-13.5,-10.0039433906299,-1.2346845122375));
#4767=CARTESIAN_POINT('Origin',(-9.5,-10.0039433906299,6.26348125396711));
#4768=CARTESIAN_POINT('',(-9.5,-10.0039433906299,6.26348125396711));
#4769=CARTESIAN_POINT('',(-13.5,-10.0039433906299,6.26348125396711));
#4770=CARTESIAN_POINT('Origin',(-13.5,0.,2.51439837086481));
#4771=CARTESIAN_POINT('Origin',(-9.5,0.,2.51439837086481));
#4772=CARTESIAN_POINT('',(0.,0.,0.));
#4773=CARTESIAN_POINT('Origin',(14.5,7.24395366693103,1.75498192028357));
#4774=CARTESIAN_POINT('',(14.5,6.24395366693103,1.75498192028357));
#4775=CARTESIAN_POINT('Origin',(14.5,7.24395366693103,1.75498192028357));
#4776=CARTESIAN_POINT('',(13.5,6.24395366693103,1.75498192028357));
#4777=CARTESIAN_POINT('',(14.5,6.24395366693103,1.75498192028357));
#4778=CARTESIAN_POINT('Origin',(13.5,7.24395366693103,1.75498192028357));
#4779=CARTESIAN_POINT('Origin',(14.5,-7.24395366693103,1.75498192028357));
#4780=CARTESIAN_POINT('',(14.5,-8.24395366693103,1.75498192028357));
#4781=CARTESIAN_POINT('Origin',(14.5,-7.24395366693103,1.75498192028357));
#4782=CARTESIAN_POINT('',(13.5,-8.24395366693103,1.75498192028357));
#4783=CARTESIAN_POINT('',(14.5,-8.24395366693103,1.75498192028357));
#4784=CARTESIAN_POINT('Origin',(13.5,-7.24395366693103,1.75498192028357));
#4785=CARTESIAN_POINT('Origin',(13.5,10.0039433906299,-1.2346845122375));
#4786=CARTESIAN_POINT('',(13.5,10.0039433906299,-1.2346845122375));
#4787=CARTESIAN_POINT('',(13.5,10.0039433906299,6.26348125396711));
#4788=CARTESIAN_POINT('',(13.5,10.0039433906299,-1.2346845122375));
#4789=CARTESIAN_POINT('',(14.5,10.0039433906299,6.26348125396711));
#4790=CARTESIAN_POINT('',(13.5,10.0039433906299,6.26348125396711));
#4791=CARTESIAN_POINT('',(14.5,10.0039433906299,-1.2346845122375));
#4792=CARTESIAN_POINT('',(14.5,10.0039433906299,-1.2346845122375));
#4793=CARTESIAN_POINT('',(13.5,10.0039433906299,-1.2346845122375));
#4794=CARTESIAN_POINT('Origin',(13.5,4.48396394323217,-1.2346845122375));
#4795=CARTESIAN_POINT('',(13.5,4.48396394323217,-1.2346845122375));
#4796=CARTESIAN_POINT('',(13.5,4.48396394323217,-1.2346845122375));
#4797=CARTESIAN_POINT('',(14.5,4.48396394323217,-1.2346845122375));
#4798=CARTESIAN_POINT('',(14.5,4.48396394323217,-1.2346845122375));
#4799=CARTESIAN_POINT('',(13.5,4.48396394323217,-1.2346845122375));
#4800=CARTESIAN_POINT('Origin',(13.5,4.48396394323217,3.23022961141938));
#4801=CARTESIAN_POINT('',(13.5,4.48396394323217,3.23022961141938));
#4802=CARTESIAN_POINT('',(13.5,4.48396394323217,3.23022961141938));
#4803=CARTESIAN_POINT('',(14.5,4.48396394323217,3.23022961141938));
#4804=CARTESIAN_POINT('',(14.5,4.48396394323217,3.23022961141938));
#4805=CARTESIAN_POINT('',(13.5,4.48396394323217,3.23022961141938));
#4806=CARTESIAN_POINT('Origin',(13.5,-4.48396394323217,3.23022961141938));
#4807=CARTESIAN_POINT('',(13.5,-4.48396394323217,3.23022961141938));
#4808=CARTESIAN_POINT('',(13.5,-4.48396394323217,3.23022961141938));
#4809=CARTESIAN_POINT('',(14.5,-4.48396394323217,3.23022961141938));
#4810=CARTESIAN_POINT('',(14.5,-4.48396394323217,3.23022961141938));
#4811=CARTESIAN_POINT('',(13.5,-4.48396394323217,3.23022961141938));
#4812=CARTESIAN_POINT('Origin',(13.5,-4.48396394323217,-1.2346845122375));
#4813=CARTESIAN_POINT('',(13.5,-4.48396394323217,-1.2346845122375));
#4814=CARTESIAN_POINT('',(13.5,-4.48396394323217,-1.2346845122375));
#4815=CARTESIAN_POINT('',(14.5,-4.48396394323217,-1.2346845122375));
#4816=CARTESIAN_POINT('',(14.5,-4.48396394323217,-1.2346845122375));
#4817=CARTESIAN_POINT('',(13.5,-4.48396394323217,-1.2346845122375));
#4818=CARTESIAN_POINT('Origin',(13.5,-10.0039433906299,-1.2346845122375));
#4819=CARTESIAN_POINT('',(13.5,-10.0039433906299,-1.2346845122375));
#4820=CARTESIAN_POINT('',(13.5,-10.0039433906299,-1.2346845122375));
#4821=CARTESIAN_POINT('',(14.5,-10.0039433906299,-1.2346845122375));
#4822=CARTESIAN_POINT('',(14.5,-10.0039433906299,-1.2346845122375));
#4823=CARTESIAN_POINT('',(13.5,-10.0039433906299,-1.2346845122375));
#4824=CARTESIAN_POINT('Origin',(13.5,-10.0039433906299,6.26348125396711));
#4825=CARTESIAN_POINT('',(13.5,-10.0039433906299,6.26348125396711));
#4826=CARTESIAN_POINT('',(13.5,-10.0039433906299,6.26348125396711));
#4827=CARTESIAN_POINT('',(14.5,-10.0039433906299,6.26348125396711));
#4828=CARTESIAN_POINT('',(14.5,-10.0039433906299,6.26348125396711));
#4829=CARTESIAN_POINT('',(13.5,-10.0039433906299,6.26348125396711));
#4830=CARTESIAN_POINT('Origin',(13.5,10.0039433906299,6.26348125396711));
#4831=CARTESIAN_POINT('',(13.5,10.0039433906299,6.26348125396711));
#4832=CARTESIAN_POINT('',(14.5,10.0039433906299,6.26348125396711));
#4833=CARTESIAN_POINT('Origin',(14.5,0.,2.51439837086481));
#4834=CARTESIAN_POINT('Origin',(13.5,0.,2.51439837086481));
#4835=CARTESIAN_POINT('',(0.,0.,0.));
#4836=CARTESIAN_POINT('Origin',(-14.5,7.24395366693103,1.75498192028357));
#4837=CARTESIAN_POINT('',(-13.5,6.24395366693103,1.75498192028357));
#4838=CARTESIAN_POINT('Origin',(-13.5,7.24395366693103,1.75498192028357));
#4839=CARTESIAN_POINT('',(-14.5,6.24395366693103,1.75498192028357));
#4840=CARTESIAN_POINT('',(-14.5,6.24395366693103,1.75498192028357));
#4841=CARTESIAN_POINT('Origin',(-14.5,7.24395366693103,1.75498192028357));
#4842=CARTESIAN_POINT('Origin',(-14.5,-7.24395366693103,1.75498192028357));
#4843=CARTESIAN_POINT('',(-13.5,-8.24395366693103,1.75498192028357));
#4844=CARTESIAN_POINT('Origin',(-13.5,-7.24395366693103,1.75498192028357));
#4845=CARTESIAN_POINT('',(-14.5,-8.24395366693103,1.75498192028357));
#4846=CARTESIAN_POINT('',(-14.5,-8.24395366693103,1.75498192028357));
#4847=CARTESIAN_POINT('Origin',(-14.5,-7.24395366693103,1.75498192028357));
#4848=CARTESIAN_POINT('Origin',(-13.5,10.0039433906299,-1.2346845122375));
#4849=CARTESIAN_POINT('',(-13.5,10.0039433906299,-1.2346845122375));
#4850=CARTESIAN_POINT('',(-13.5,10.0039433906299,6.26348125396711));
#4851=CARTESIAN_POINT('',(-13.5,10.0039433906299,-1.2346845122375));
#4852=CARTESIAN_POINT('',(-14.5,10.0039433906299,-1.2346845122375));
#4853=CARTESIAN_POINT('',(-13.5,10.0039433906299,-1.2346845122375));
#4854=CARTESIAN_POINT('',(-14.5,10.0039433906299,6.26348125396711));
#4855=CARTESIAN_POINT('',(-14.5,10.0039433906299,-1.2346845122375));
#4856=CARTESIAN_POINT('',(-13.5,10.0039433906299,6.26348125396711));
#4857=CARTESIAN_POINT('Origin',(-13.5,4.48396394323217,-1.2346845122375));
#4858=CARTESIAN_POINT('',(-13.5,4.48396394323217,-1.2346845122375));
#4859=CARTESIAN_POINT('',(-13.5,4.48396394323217,-1.2346845122375));
#4860=CARTESIAN_POINT('',(-14.5,4.48396394323217,-1.2346845122375));
#4861=CARTESIAN_POINT('',(-13.5,4.48396394323217,-1.2346845122375));
#4862=CARTESIAN_POINT('',(-14.5,4.48396394323217,-1.2346845122375));
#4863=CARTESIAN_POINT('Origin',(-13.5,4.48396394323217,3.23022961141938));
#4864=CARTESIAN_POINT('',(-13.5,4.48396394323217,3.23022961141938));
#4865=CARTESIAN_POINT('',(-13.5,4.48396394323217,3.23022961141938));
#4866=CARTESIAN_POINT('',(-14.5,4.48396394323217,3.23022961141938));
#4867=CARTESIAN_POINT('',(-13.5,4.48396394323217,3.23022961141938));
#4868=CARTESIAN_POINT('',(-14.5,4.48396394323217,3.23022961141938));
#4869=CARTESIAN_POINT('Origin',(-13.5,-4.48396394323217,3.23022961141938));
#4870=CARTESIAN_POINT('',(-13.5,-4.48396394323217,3.23022961141938));
#4871=CARTESIAN_POINT('',(-13.5,-4.48396394323217,3.23022961141938));
#4872=CARTESIAN_POINT('',(-14.5,-4.48396394323217,3.23022961141938));
#4873=CARTESIAN_POINT('',(-13.5,-4.48396394323217,3.23022961141938));
#4874=CARTESIAN_POINT('',(-14.5,-4.48396394323217,3.23022961141938));
#4875=CARTESIAN_POINT('Origin',(-13.5,-4.48396394323217,-1.2346845122375));
#4876=CARTESIAN_POINT('',(-13.5,-4.48396394323217,-1.2346845122375));
#4877=CARTESIAN_POINT('',(-13.5,-4.48396394323217,-1.2346845122375));
#4878=CARTESIAN_POINT('',(-14.5,-4.48396394323217,-1.2346845122375));
#4879=CARTESIAN_POINT('',(-13.5,-4.48396394323217,-1.2346845122375));
#4880=CARTESIAN_POINT('',(-14.5,-4.48396394323217,-1.2346845122375));
#4881=CARTESIAN_POINT('Origin',(-13.5,-10.0039433906299,-1.2346845122375));
#4882=CARTESIAN_POINT('',(-13.5,-10.0039433906299,-1.2346845122375));
#4883=CARTESIAN_POINT('',(-13.5,-10.0039433906299,-1.2346845122375));
#4884=CARTESIAN_POINT('',(-14.5,-10.0039433906299,-1.2346845122375));
#4885=CARTESIAN_POINT('',(-13.5,-10.0039433906299,-1.2346845122375));
#4886=CARTESIAN_POINT('',(-14.5,-10.0039433906299,-1.2346845122375));
#4887=CARTESIAN_POINT('Origin',(-13.5,-10.0039433906299,6.26348125396711));
#4888=CARTESIAN_POINT('',(-13.5,-10.0039433906299,6.26348125396711));
#4889=CARTESIAN_POINT('',(-13.5,-10.0039433906299,6.26348125396711));
#4890=CARTESIAN_POINT('',(-14.5,-10.0039433906299,6.26348125396711));
#4891=CARTESIAN_POINT('',(-13.5,-10.0039433906299,6.26348125396711));
#4892=CARTESIAN_POINT('',(-14.5,-10.0039433906299,6.26348125396711));
#4893=CARTESIAN_POINT('Origin',(-13.5,10.0039433906299,6.26348125396711));
#4894=CARTESIAN_POINT('',(-13.5,10.0039433906299,6.26348125396711));
#4895=CARTESIAN_POINT('',(-14.5,10.0039433906299,6.26348125396711));
#4896=CARTESIAN_POINT('Origin',(-14.5,0.,2.51439837086481));
#4897=CARTESIAN_POINT('Origin',(-13.5,0.,2.51439837086481));
#4898=CARTESIAN_POINT('',(0.,0.,0.));
#4899=CARTESIAN_POINT('Origin',(14.5,7.24395366693103,1.75498192028357));
#4900=CARTESIAN_POINT('',(13.5,6.24395366693103,1.75498192028357));
#4901=CARTESIAN_POINT('Origin',(13.5,7.24395366693103,1.75498192028357));
#4902=CARTESIAN_POINT('',(9.5,6.24395366693103,1.75498192028357));
#4903=CARTESIAN_POINT('',(14.5,6.24395366693103,1.75498192028357));
#4904=CARTESIAN_POINT('Origin',(9.5,7.24395366693103,1.75498192028357));
#4905=CARTESIAN_POINT('Origin',(14.5,-7.24395366693103,1.75498192028357));
#4906=CARTESIAN_POINT('',(13.5,-8.24395366693103,1.75498192028357));
#4907=CARTESIAN_POINT('Origin',(13.5,-7.24395366693103,1.75498192028357));
#4908=CARTESIAN_POINT('',(9.5,-8.24395366693103,1.75498192028357));
#4909=CARTESIAN_POINT('',(14.5,-8.24395366693103,1.75498192028357));
#4910=CARTESIAN_POINT('Origin',(9.5,-7.24395366693103,1.75498192028357));
#4911=CARTESIAN_POINT('Origin',(9.5,10.0039433906299,6.26348125396711));
#4912=CARTESIAN_POINT('',(9.5,10.0039433906299,6.26348125396711));
#4913=CARTESIAN_POINT('',(9.5,-10.0039433906299,6.26348125396711));
#4914=CARTESIAN_POINT('',(9.5,10.0039433906299,6.26348125396711));
#4915=CARTESIAN_POINT('',(13.5,-10.0039433906299,6.26348125396711));
#4916=CARTESIAN_POINT('',(9.5,-10.0039433906299,6.26348125396711));
#4917=CARTESIAN_POINT('',(13.5,10.0039433906299,6.26348125396711));
#4918=CARTESIAN_POINT('',(13.5,10.0039433906299,6.26348125396711));
#4919=CARTESIAN_POINT('',(9.5,10.0039433906299,6.26348125396711));
#4920=CARTESIAN_POINT('Origin',(9.5,10.0039433906299,-1.2346845122375));
#4921=CARTESIAN_POINT('',(9.5,10.0039433906299,-1.2346845122375));
#4922=CARTESIAN_POINT('',(9.5,10.0039433906299,-1.2346845122375));
#4923=CARTESIAN_POINT('',(13.5,10.0039433906299,-1.2346845122375));
#4924=CARTESIAN_POINT('',(13.5,10.0039433906299,-1.2346845122375));
#4925=CARTESIAN_POINT('',(9.5,10.0039433906299,-1.2346845122375));
#4926=CARTESIAN_POINT('Origin',(9.5,4.48396394323217,-1.2346845122375));
#4927=CARTESIAN_POINT('',(9.5,4.48396394323217,-1.2346845122375));
#4928=CARTESIAN_POINT('',(9.5,-10.0039433906299,-1.2346845122375));
#4929=CARTESIAN_POINT('',(13.5,4.48396394323217,-1.2346845122375));
#4930=CARTESIAN_POINT('',(13.5,-10.0039433906299,-1.2346845122375));
#4931=CARTESIAN_POINT('',(9.5,4.48396394323217,-1.2346845122375));
#4932=CARTESIAN_POINT('Origin',(9.5,4.48396394323217,3.23022961141938));
#4933=CARTESIAN_POINT('',(9.5,4.48396394323217,3.23022961141938));
#4934=CARTESIAN_POINT('',(9.5,4.48396394323217,3.23022961141938));
#4935=CARTESIAN_POINT('',(13.5,4.48396394323217,3.23022961141938));
#4936=CARTESIAN_POINT('',(13.5,4.48396394323217,3.23022961141938));
#4937=CARTESIAN_POINT('',(9.5,4.48396394323217,3.23022961141938));
#4938=CARTESIAN_POINT('Origin',(9.5,-4.48396394323217,3.23022961141938));
#4939=CARTESIAN_POINT('',(9.5,-4.48396394323217,3.23022961141938));
#4940=CARTESIAN_POINT('',(9.5,-4.48396394323217,3.23022961141938));
#4941=CARTESIAN_POINT('',(13.5,-4.48396394323217,3.23022961141938));
#4942=CARTESIAN_POINT('',(13.5,-4.48396394323217,3.23022961141938));
#4943=CARTESIAN_POINT('',(9.5,-4.48396394323217,3.23022961141938));
#4944=CARTESIAN_POINT('Origin',(9.5,-4.48396394323217,-1.2346845122375));
#4945=CARTESIAN_POINT('',(9.5,-4.48396394323217,-1.2346845122375));
#4946=CARTESIAN_POINT('',(9.5,-4.48396394323217,-1.2346845122375));
#4947=CARTESIAN_POINT('',(13.5,-4.48396394323217,-1.2346845122375));
#4948=CARTESIAN_POINT('',(13.5,-4.48396394323217,-1.2346845122375));
#4949=CARTESIAN_POINT('',(9.5,-4.48396394323217,-1.2346845122375));
#4950=CARTESIAN_POINT('Origin',(9.5,-10.0039433906299,-1.2346845122375));
#4951=CARTESIAN_POINT('',(9.5,-10.0039433906299,-1.2346845122375));
#4952=CARTESIAN_POINT('',(9.5,-10.0039433906299,-1.2346845122375));
#4953=CARTESIAN_POINT('',(13.5,-10.0039433906299,-1.2346845122375));
#4954=CARTESIAN_POINT('',(13.5,-10.0039433906299,-1.2346845122375));
#4955=CARTESIAN_POINT('',(9.5,-10.0039433906299,-1.2346845122375));
#4956=CARTESIAN_POINT('Origin',(9.5,-10.0039433906299,6.26348125396711));
#4957=CARTESIAN_POINT('',(9.5,-10.0039433906299,6.26348125396711));
#4958=CARTESIAN_POINT('',(13.5,-10.0039433906299,6.26348125396711));
#4959=CARTESIAN_POINT('Origin',(13.5,0.,2.51439837086481));
#4960=CARTESIAN_POINT('Origin',(9.5,0.,2.51439837086481));
#4961=CARTESIAN_POINT('',(14.5,7.24395366693103,1.75498192028357));
#4962=CARTESIAN_POINT('',(14.5,-7.24395366693103,1.75498192028357));
#4963=CARTESIAN_POINT('',(-14.5,7.24395366693103,1.75498192028357));
#4964=CARTESIAN_POINT('',(-14.5,-7.24395366693103,1.75498192028357));
#4965=CARTESIAN_POINT('',(0.,0.,0.));
#4966=CARTESIAN_POINT('',(0.,0.,0.));
#4967=CARTESIAN_POINT('',(0.,0.,0.));
#4968=CARTESIAN_POINT('',(0.,0.,0.));
#4969=CARTESIAN_POINT('',(0.,0.,0.));
#4970=CARTESIAN_POINT('',(0.,0.,0.));
#4971=UNCERTAINTY_MEASURE_WITH_UNIT(LENGTH_MEASURE(0.01),#4995,
'DISTANCE_ACCURACY_VALUE',
'Maximum model space distance between geometric entities at asserted c
onnectivities');
#4972=UNCERTAINTY_MEASURE_WITH_UNIT(LENGTH_MEASURE(0.01),#4995,
'DISTANCE_ACCURACY_VALUE',
'Maximum model space distance between geometric entities at asserted c
onnectivities');
#4973=UNCERTAINTY_MEASURE_WITH_UNIT(LENGTH_MEASURE(0.01),#4995,
'DISTANCE_ACCURACY_VALUE',
'Maximum model space distance between geometric entities at asserted c
onnectivities');
#4974=UNCERTAINTY_MEASURE_WITH_UNIT(LENGTH_MEASURE(0.01),#4995,
'DISTANCE_ACCURACY_VALUE',
'Maximum model space distance between geometric entities at asserted c
onnectivities');
#4975=UNCERTAINTY_MEASURE_WITH_UNIT(LENGTH_MEASURE(0.01),#4995,
'DISTANCE_ACCURACY_VALUE',
'Maximum model space distance between geometric entities at asserted c
onnectivities');
#4976=UNCERTAINTY_MEASURE_WITH_UNIT(LENGTH_MEASURE(0.01),#4995,
'DISTANCE_ACCURACY_VALUE',
'Maximum model space distance between geometric entities at asserted c
onnectivities');
#4977=UNCERTAINTY_MEASURE_WITH_UNIT(LENGTH_MEASURE(0.01),#4995,
'DISTANCE_ACCURACY_VALUE',
'Maximum model space distance between geometric entities at asserted c
onnectivities');
#4978=UNCERTAINTY_MEASURE_WITH_UNIT(LENGTH_MEASURE(0.01),#4995,
'DISTANCE_ACCURACY_VALUE',
'Maximum model space distance between geometric entities at asserted c
onnectivities');
#4979=UNCERTAINTY_MEASURE_WITH_UNIT(LENGTH_MEASURE(0.01),#4995,
'DISTANCE_ACCURACY_VALUE',
'Maximum model space distance between geometric entities at asserted c
onnectivities');
#4980=UNCERTAINTY_MEASURE_WITH_UNIT(LENGTH_MEASURE(0.01),#4995,
'DISTANCE_ACCURACY_VALUE',
'Maximum model space distance between geometric entities at asserted c
onnectivities');
#4981=UNCERTAINTY_MEASURE_WITH_UNIT(LENGTH_MEASURE(0.01),#4995,
'DISTANCE_ACCURACY_VALUE',
'Maximum model space distance between geometric entities at asserted c
onnectivities');
#4982=UNCERTAINTY_MEASURE_WITH_UNIT(LENGTH_MEASURE(0.01),#4995,
'DISTANCE_ACCURACY_VALUE',
'Maximum model space distance between geometric entities at asserted c
onnectivities');
#4983=(
GEOMETRIC_REPRESENTATION_CONTEXT(3)
GLOBAL_UNCERTAINTY_ASSIGNED_CONTEXT((#4971))
GLOBAL_UNIT_ASSIGNED_CONTEXT((#4995,#4997,#4998))
REPRESENTATION_CONTEXT('','3D')
);
#4984=(
GEOMETRIC_REPRESENTATION_CONTEXT(3)
GLOBAL_UNCERTAINTY_ASSIGNED_CONTEXT((#4972))
GLOBAL_UNIT_ASSIGNED_CONTEXT((#4995,#4997,#4998))
REPRESENTATION_CONTEXT('','3D')
);
#4985=(
GEOMETRIC_REPRESENTATION_CONTEXT(3)
GLOBAL_UNCERTAINTY_ASSIGNED_CONTEXT((#4973))
GLOBAL_UNIT_ASSIGNED_CONTEXT((#4995,#4997,#4998))
REPRESENTATION_CONTEXT('','3D')
);
#4986=(
GEOMETRIC_REPRESENTATION_CONTEXT(3)
GLOBAL_UNCERTAINTY_ASSIGNED_CONTEXT((#4974))
GLOBAL_UNIT_ASSIGNED_CONTEXT((#4995,#4997,#4998))
REPRESENTATION_CONTEXT('','3D')
);
#4987=(
GEOMETRIC_REPRESENTATION_CONTEXT(3)
GLOBAL_UNCERTAINTY_ASSIGNED_CONTEXT((#4975))
GLOBAL_UNIT_ASSIGNED_CONTEXT((#4995,#4997,#4998))
REPRESENTATION_CONTEXT('','3D')
);
#4988=(
GEOMETRIC_REPRESENTATION_CONTEXT(3)
GLOBAL_UNCERTAINTY_ASSIGNED_CONTEXT((#4976))
GLOBAL_UNIT_ASSIGNED_CONTEXT((#4995,#4997,#4998))
REPRESENTATION_CONTEXT('','3D')
);
#4989=(
GEOMETRIC_REPRESENTATION_CONTEXT(3)
GLOBAL_UNCERTAINTY_ASSIGNED_CONTEXT((#4977))
GLOBAL_UNIT_ASSIGNED_CONTEXT((#4995,#4997,#4998))
REPRESENTATION_CONTEXT('','3D')
);
#4990=(
GEOMETRIC_REPRESENTATION_CONTEXT(3)
GLOBAL_UNCERTAINTY_ASSIGNED_CONTEXT((#4978))
GLOBAL_UNIT_ASSIGNED_CONTEXT((#4995,#4997,#4998))
REPRESENTATION_CONTEXT('','3D')
);
#4991=(
GEOMETRIC_REPRESENTATION_CONTEXT(3)
GLOBAL_UNCERTAINTY_ASSIGNED_CONTEXT((#4979))
GLOBAL_UNIT_ASSIGNED_CONTEXT((#4995,#4997,#4998))
REPRESENTATION_CONTEXT('','3D')
);
#4992=(
GEOMETRIC_REPRESENTATION_CONTEXT(3)
GLOBAL_UNCERTAINTY_ASSIGNED_CONTEXT((#4980))
GLOBAL_UNIT_ASSIGNED_CONTEXT((#4995,#4997,#4998))
REPRESENTATION_CONTEXT('','3D')
);
#4993=(
GEOMETRIC_REPRESENTATION_CONTEXT(3)
GLOBAL_UNCERTAINTY_ASSIGNED_CONTEXT((#4981))
GLOBAL_UNIT_ASSIGNED_CONTEXT((#4995,#4997,#4998))
REPRESENTATION_CONTEXT('','3D')
);
#4994=(
GEOMETRIC_REPRESENTATION_CONTEXT(3)
GLOBAL_UNCERTAINTY_ASSIGNED_CONTEXT((#4982))
GLOBAL_UNIT_ASSIGNED_CONTEXT((#4995,#4997,#4998))
REPRESENTATION_CONTEXT('','3D')
);
#4995=(
LENGTH_UNIT()
NAMED_UNIT(*)
SI_UNIT(.MILLI.,.METRE.)
);
#4996=(
LENGTH_UNIT()
NAMED_UNIT(*)
SI_UNIT($,.METRE.)
);
#4997=(
NAMED_UNIT(*)
PLANE_ANGLE_UNIT()
SI_UNIT($,.RADIAN.)
);
#4998=(
NAMED_UNIT(*)
SI_UNIT($,.STERADIAN.)
SOLID_ANGLE_UNIT()
);
#4999=SHAPE_DEFINITION_REPRESENTATION(#5010,#5031);
#5000=SHAPE_DEFINITION_REPRESENTATION(#5011,#5032);
#5001=SHAPE_DEFINITION_REPRESENTATION(#5012,#5033);
#5002=SHAPE_DEFINITION_REPRESENTATION(#5013,#5034);
#5003=SHAPE_DEFINITION_REPRESENTATION(#5014,#5035);
#5004=SHAPE_DEFINITION_REPRESENTATION(#5015,#5036);
#5005=SHAPE_DEFINITION_REPRESENTATION(#5016,#5037);
#5006=SHAPE_DEFINITION_REPRESENTATION(#5017,#5038);
#5007=SHAPE_DEFINITION_REPRESENTATION(#5018,#5039);
#5008=SHAPE_DEFINITION_REPRESENTATION(#5019,#5040);
#5009=SHAPE_DEFINITION_REPRESENTATION(#5020,#5041);
#5010=PRODUCT_DEFINITION_SHAPE('',$,#5043);
#5011=PRODUCT_DEFINITION_SHAPE('',$,#5044);
#5012=PRODUCT_DEFINITION_SHAPE('',$,#5045);
#5013=PRODUCT_DEFINITION_SHAPE('',$,#5046);
#5014=PRODUCT_DEFINITION_SHAPE('',$,#5047);
#5015=PRODUCT_DEFINITION_SHAPE('',$,#5048);
#5016=PRODUCT_DEFINITION_SHAPE('',$,#5049);
#5017=PRODUCT_DEFINITION_SHAPE('',$,#5050);
#5018=PRODUCT_DEFINITION_SHAPE('',$,#5051);
#5019=PRODUCT_DEFINITION_SHAPE('',$,#5052);
#5020=PRODUCT_DEFINITION_SHAPE('',$,#5053);
#5021=PRODUCT_DEFINITION_SHAPE($,$,#41);
#5022=PRODUCT_DEFINITION_SHAPE($,$,#42);
#5023=PRODUCT_DEFINITION_SHAPE($,$,#43);
#5024=PRODUCT_DEFINITION_SHAPE($,$,#44);
#5025=PRODUCT_DEFINITION_SHAPE($,$,#45);
#5026=PRODUCT_DEFINITION_SHAPE($,$,#46);
#5027=PRODUCT_DEFINITION_SHAPE($,$,#47);
#5028=PRODUCT_DEFINITION_SHAPE($,$,#48);
#5029=PRODUCT_DEFINITION_SHAPE($,$,#49);
#5030=PRODUCT_DEFINITION_SHAPE($,$,#50);
#5031=SHAPE_REPRESENTATION('',(#3032,#3302,#3303,#3304,#3305,#3306,#3307,
#3308,#3309,#3310,#3311),#4983);
#5032=SHAPE_REPRESENTATION('',(#3033),#4984);
#5033=SHAPE_REPRESENTATION('',(#3060),#4985);
#5034=SHAPE_REPRESENTATION('',(#3087),#4986);
#5035=SHAPE_REPRESENTATION('',(#3114),#4987);
#5036=SHAPE_REPRESENTATION('',(#3141),#4988);
#5037=SHAPE_REPRESENTATION('',(#3203),#4989);
#5038=SHAPE_REPRESENTATION('',(#3234),#4990);
#5039=SHAPE_REPRESENTATION('',(#3251),#4991);
#5040=SHAPE_REPRESENTATION('',(#3268),#4992);
#5041=SHAPE_REPRESENTATION('',(#3285),#4993);
#5042=PRODUCT_DEFINITION_CONTEXT('part definition',#5077,'design');
#5043=PRODUCT_DEFINITION('BR-352','BR-352',#5054,#5042);
#5044=PRODUCT_DEFINITION(
'BSHCS ASME B18.3.1M - M2x0.4 x 5 Steel Grade 2 Plain','Screw_01',#5055,
#5042);
#5045=PRODUCT_DEFINITION(
'BSHCS ASME B18.3.1M - M2x0.4 x 5 Steel Grade 2 Plain_1','Screw_02',#5056,
#5042);
#5046=PRODUCT_DEFINITION(
'BSHCS ASME B18.3.1M - M2x0.4 x 5 Steel Grade 2 Plain_2','Screw_03',#5057,
#5042);
#5047=PRODUCT_DEFINITION(
'BSHCS ASME B18.3.1M - M2x0.4 x 5 Steel Grade 2 Plain_3','Screw_04',#5058,
#5042);
#5048=PRODUCT_DEFINITION('Rail','Rail',#5059,#5042);
#5049=PRODUCT_DEFINITION('Carriage','Carriage',#5060,#5042);
#5050=PRODUCT_DEFINITION('Middle_Part_02','Middle_Part_02',#5061,#5042);
#5051=PRODUCT_DEFINITION('End_Cap_01','End_Cap_01',#5062,#5042);
#5052=PRODUCT_DEFINITION('End_Cap_02','End_Cap_02',#5063,#5042);
#5053=PRODUCT_DEFINITION('Middle_Part_01','Middle_Part_01',#5064,#5042);
#5054=PRODUCT_DEFINITION_FORMATION('',$,#5079);
#5055=PRODUCT_DEFINITION_FORMATION('',$,#5080);
#5056=PRODUCT_DEFINITION_FORMATION('',$,#5081);
#5057=PRODUCT_DEFINITION_FORMATION('',$,#5082);
#5058=PRODUCT_DEFINITION_FORMATION('',$,#5083);
#5059=PRODUCT_DEFINITION_FORMATION('',$,#5084);
#5060=PRODUCT_DEFINITION_FORMATION('',$,#5085);
#5061=PRODUCT_DEFINITION_FORMATION('',$,#5086);
#5062=PRODUCT_DEFINITION_FORMATION('',$,#5087);
#5063=PRODUCT_DEFINITION_FORMATION('',$,#5088);
#5064=PRODUCT_DEFINITION_FORMATION('',$,#5089);
#5065=PRODUCT_RELATED_PRODUCT_CATEGORY('BR-352','BR-352',(#5079));
#5066=PRODUCT_RELATED_PRODUCT_CATEGORY('Screw_01','Screw_01',(#5080));
#5067=PRODUCT_RELATED_PRODUCT_CATEGORY('Screw_02','Screw_02',(#5081));
#5068=PRODUCT_RELATED_PRODUCT_CATEGORY('Screw_03','Screw_03',(#5082));
#5069=PRODUCT_RELATED_PRODUCT_CATEGORY('Screw_04','Screw_04',(#5083));
#5070=PRODUCT_RELATED_PRODUCT_CATEGORY('Rail','Rail',(#5084));
#5071=PRODUCT_RELATED_PRODUCT_CATEGORY('Carriage','Carriage',(#5085));
#5072=PRODUCT_RELATED_PRODUCT_CATEGORY('Middle_Part_02',
'Middle_Part_02',(#5086));
#5073=PRODUCT_RELATED_PRODUCT_CATEGORY('End_Cap_01','End_Cap_01',(#5087));
#5074=PRODUCT_RELATED_PRODUCT_CATEGORY('End_Cap_02','End_Cap_02',(#5088));
#5075=PRODUCT_RELATED_PRODUCT_CATEGORY('Middle_Part_01',
'Middle_Part_01',(#5089));
#5076=APPLICATION_PROTOCOL_DEFINITION('international standard',
'automotive_design',2009,#5077);
#5077=APPLICATION_CONTEXT(
'Core Data for Automotive Mechanical Design Process');
#5078=PRODUCT_CONTEXT('part definition',#5077,'mechanical');
#5079=PRODUCT('BR-352','BR-352',$,(#5078));
#5080=PRODUCT('BSHCS ASME B18.3.1M - M2x0.4 x 5 Steel Grade 2 Plain',
'Screw_01',
'Broached Hexagon Socket Head Cap Screw ASME B18.3.1M - M2x0.4 x 5',(#5078));
#5081=PRODUCT('BSHCS ASME B18.3.1M - M2x0.4 x 5 Steel Grade 2 Plain_1',
'Screw_02',
'Broached Hexagon Socket Head Cap Screw ASME B18.3.1M - M2x0.4 x 5',(#5078));
#5082=PRODUCT('BSHCS ASME B18.3.1M - M2x0.4 x 5 Steel Grade 2 Plain_2',
'Screw_03',
'Broached Hexagon Socket Head Cap Screw ASME B18.3.1M - M2x0.4 x 5',(#5078));
#5083=PRODUCT('BSHCS ASME B18.3.1M - M2x0.4 x 5 Steel Grade 2 Plain_3',
'Screw_04',
'Broached Hexagon Socket Head Cap Screw ASME B18.3.1M - M2x0.4 x 5',(#5078));
#5084=PRODUCT('Rail','Rail',$,(#5078));
#5085=PRODUCT('Carriage','Carriage',$,(#5078));
#5086=PRODUCT('Middle_Part_02','Middle_Part_02',$,(#5078));
#5087=PRODUCT('End_Cap_01','End_Cap_01',$,(#5078));
#5088=PRODUCT('End_Cap_02','End_Cap_02',$,(#5078));
#5089=PRODUCT('Middle_Part_01','Middle_Part_01',$,(#5078));
#5090=PRESENTATION_STYLE_ASSIGNMENT((#5095));
#5091=PRESENTATION_STYLE_ASSIGNMENT((#5096));
#5092=PRESENTATION_STYLE_ASSIGNMENT((#5097));
#5093=PRESENTATION_STYLE_ASSIGNMENT((#5098));
#5094=PRESENTATION_STYLE_ASSIGNMENT((#5099));
#5095=SURFACE_STYLE_USAGE(.BOTH.,#5100);
#5096=SURFACE_STYLE_USAGE(.BOTH.,#5101);
#5097=SURFACE_STYLE_USAGE(.BOTH.,#5102);
#5098=SURFACE_STYLE_USAGE(.BOTH.,#5103);
#5099=SURFACE_STYLE_USAGE(.BOTH.,#5104);
#5100=SURFACE_SIDE_STYLE('',(#5105));
#5101=SURFACE_SIDE_STYLE('',(#5106));
#5102=SURFACE_SIDE_STYLE('',(#5107));
#5103=SURFACE_SIDE_STYLE('',(#5108));
#5104=SURFACE_SIDE_STYLE('',(#5109));
#5105=SURFACE_STYLE_FILL_AREA(#5110);
#5106=SURFACE_STYLE_FILL_AREA(#5111);
#5107=SURFACE_STYLE_FILL_AREA(#5112);
#5108=SURFACE_STYLE_FILL_AREA(#5113);
#5109=SURFACE_STYLE_FILL_AREA(#5114);
#5110=FILL_AREA_STYLE('Steel - Satin',(#5115));
#5111=FILL_AREA_STYLE('Opaque(160,160,160)',(#5116));
#5112=FILL_AREA_STYLE('Opaque(211,211,211)',(#5117));
#5113=FILL_AREA_STYLE('Opaque(70,70,209)',(#5118));
#5114=FILL_AREA_STYLE('Opaque(196,0,0)',(#5119));
#5115=FILL_AREA_STYLE_COLOUR('Steel - Satin',#5120);
#5116=FILL_AREA_STYLE_COLOUR('Opaque(160,160,160)',#5121);
#5117=FILL_AREA_STYLE_COLOUR('Opaque(211,211,211)',#5122);
#5118=FILL_AREA_STYLE_COLOUR('Opaque(70,70,209)',#5123);
#5119=FILL_AREA_STYLE_COLOUR('Opaque(196,0,0)',#5124);
#5120=COLOUR_RGB('Steel - Satin', 0.09019608, 0.27058824, 0.51372549);
#5121=COLOUR_RGB('Opaque(160,160,160)', 0.09019608, 0.27058824, 0.51372549);
#5122=COLOUR_RGB('Opaque(211,211,211)', 0.72549020, 0.75294118, 0.79215686);
#5123=COLOUR_RGB('Opaque(70,70,209)', 0.09019608, 0.27058824, 0.51372549);
#5124=COLOUR_RGB('Opaque(196,0,0)', 0.66274510, 0.83137255, 0.94901961);
ENDSEC;
END-ISO-10303-21;
